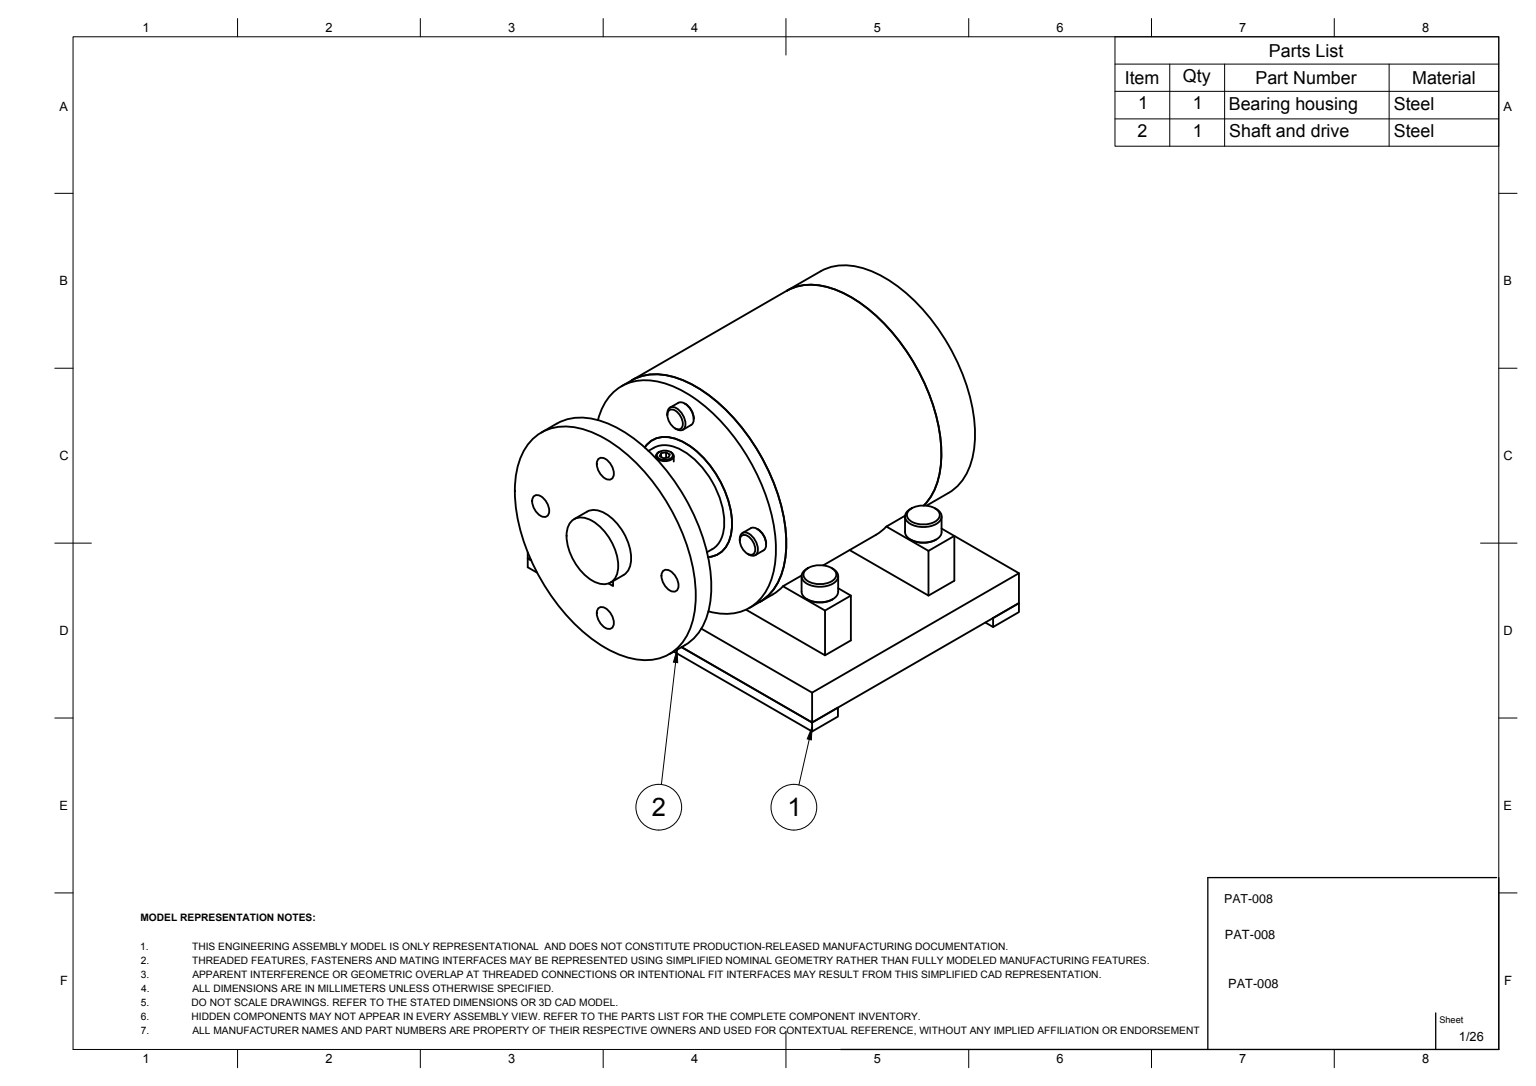
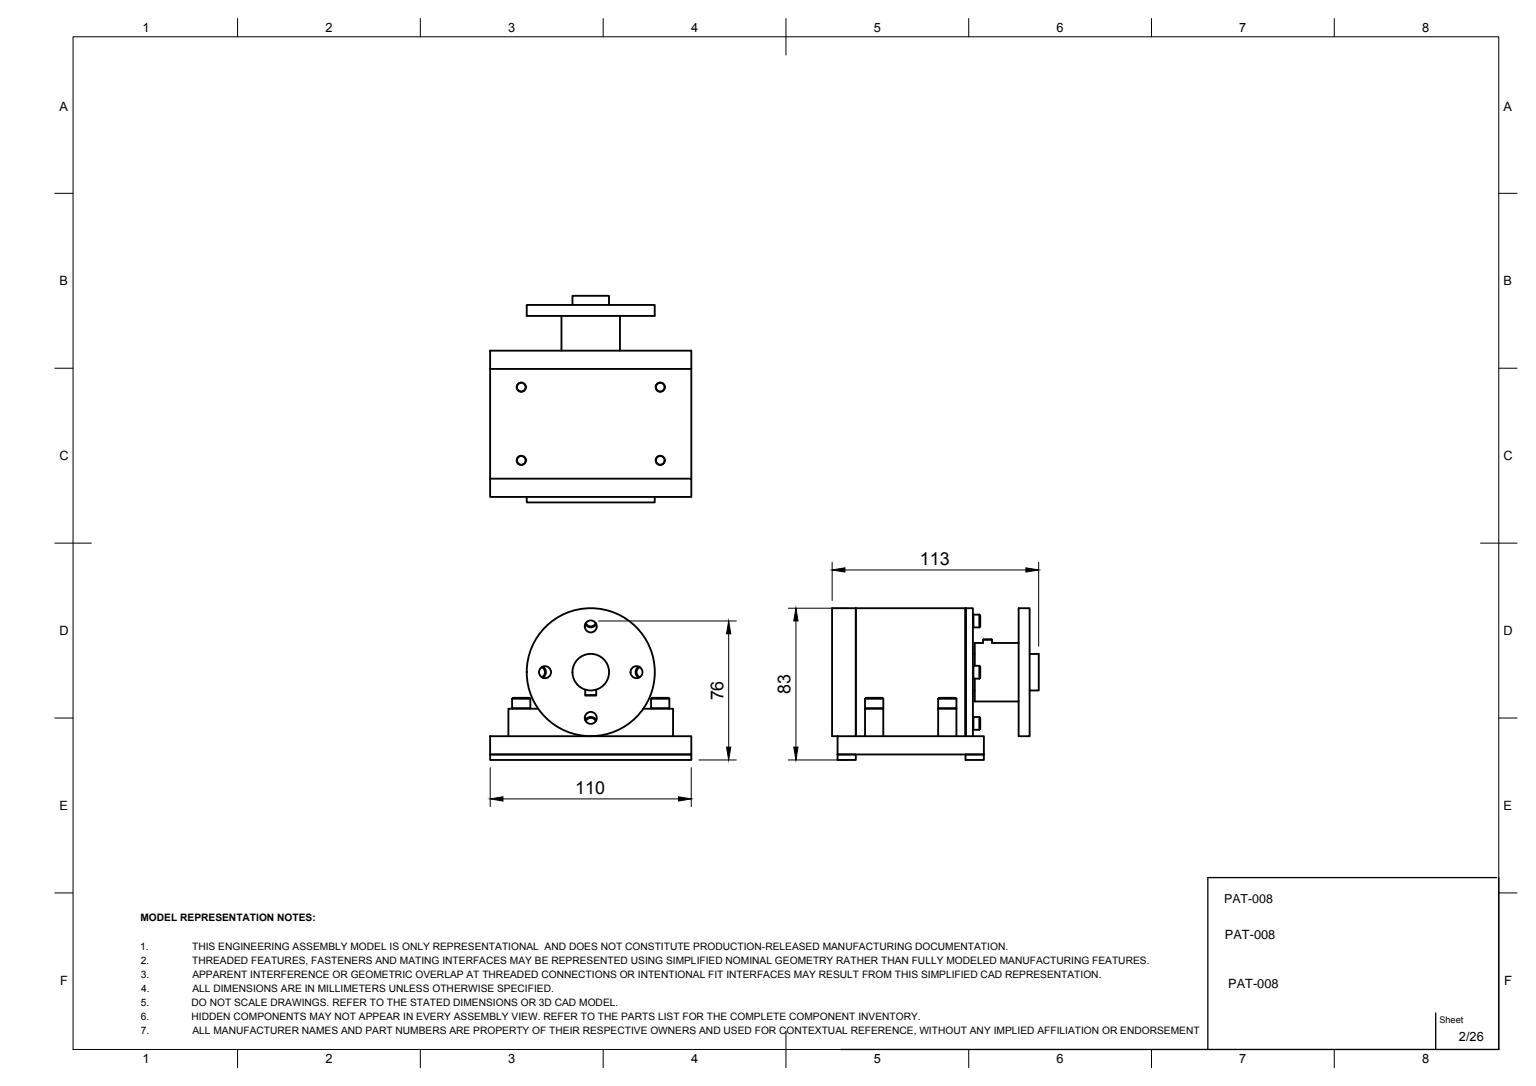
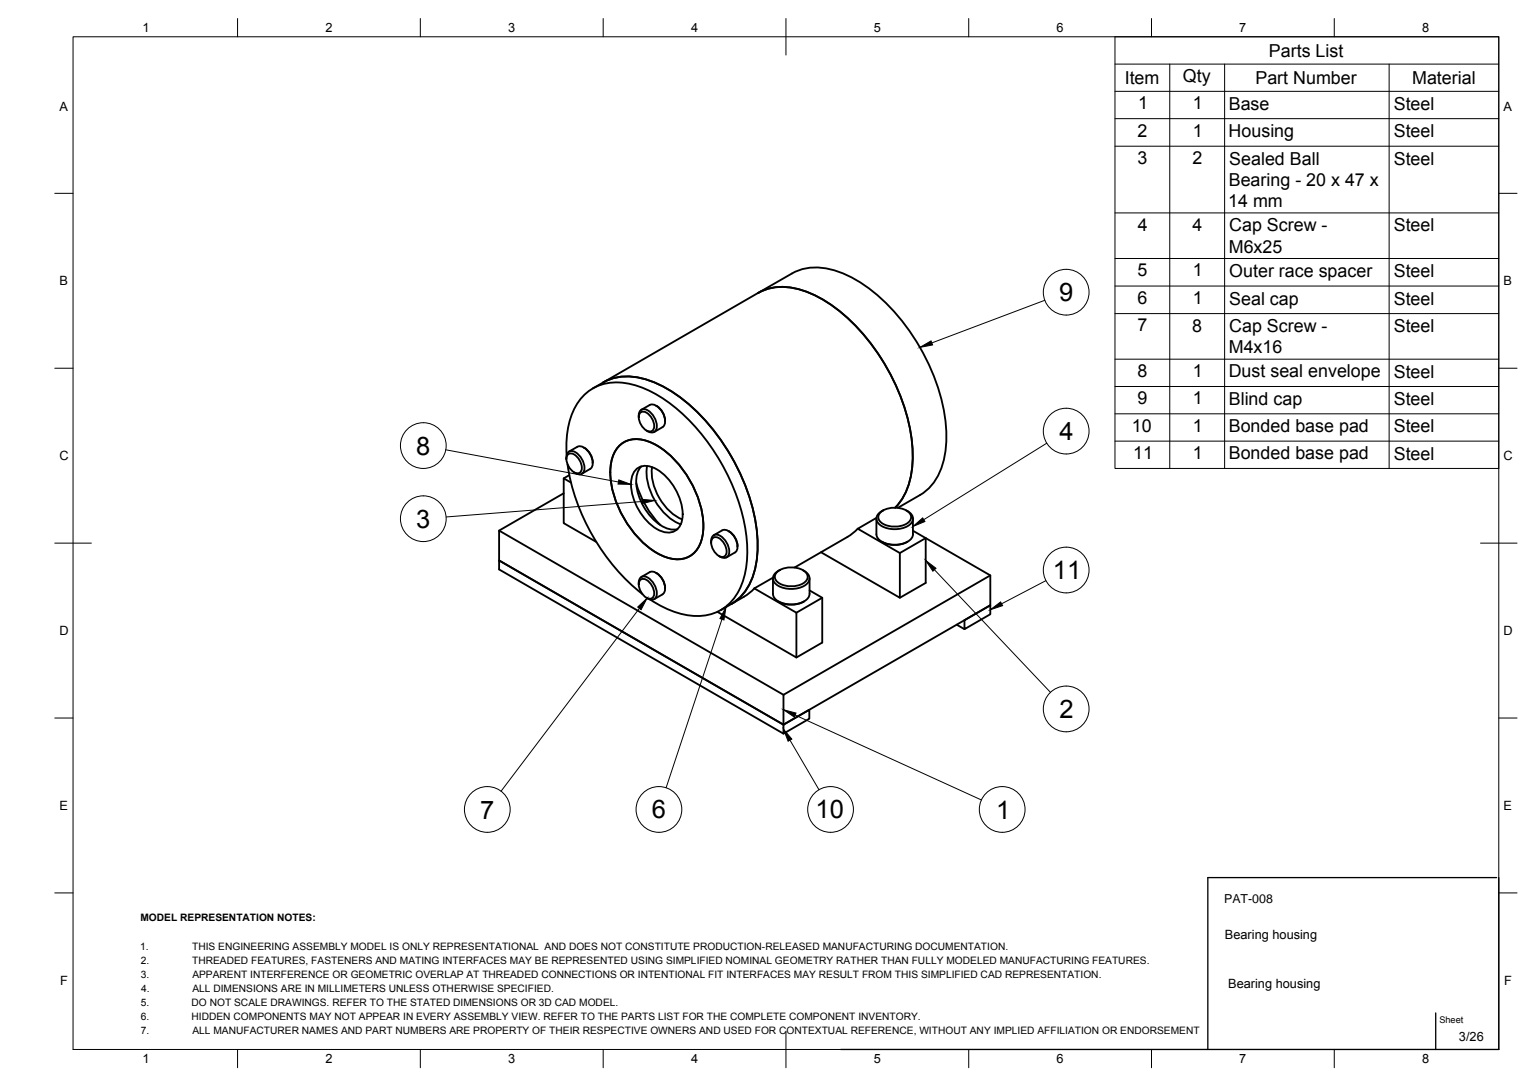
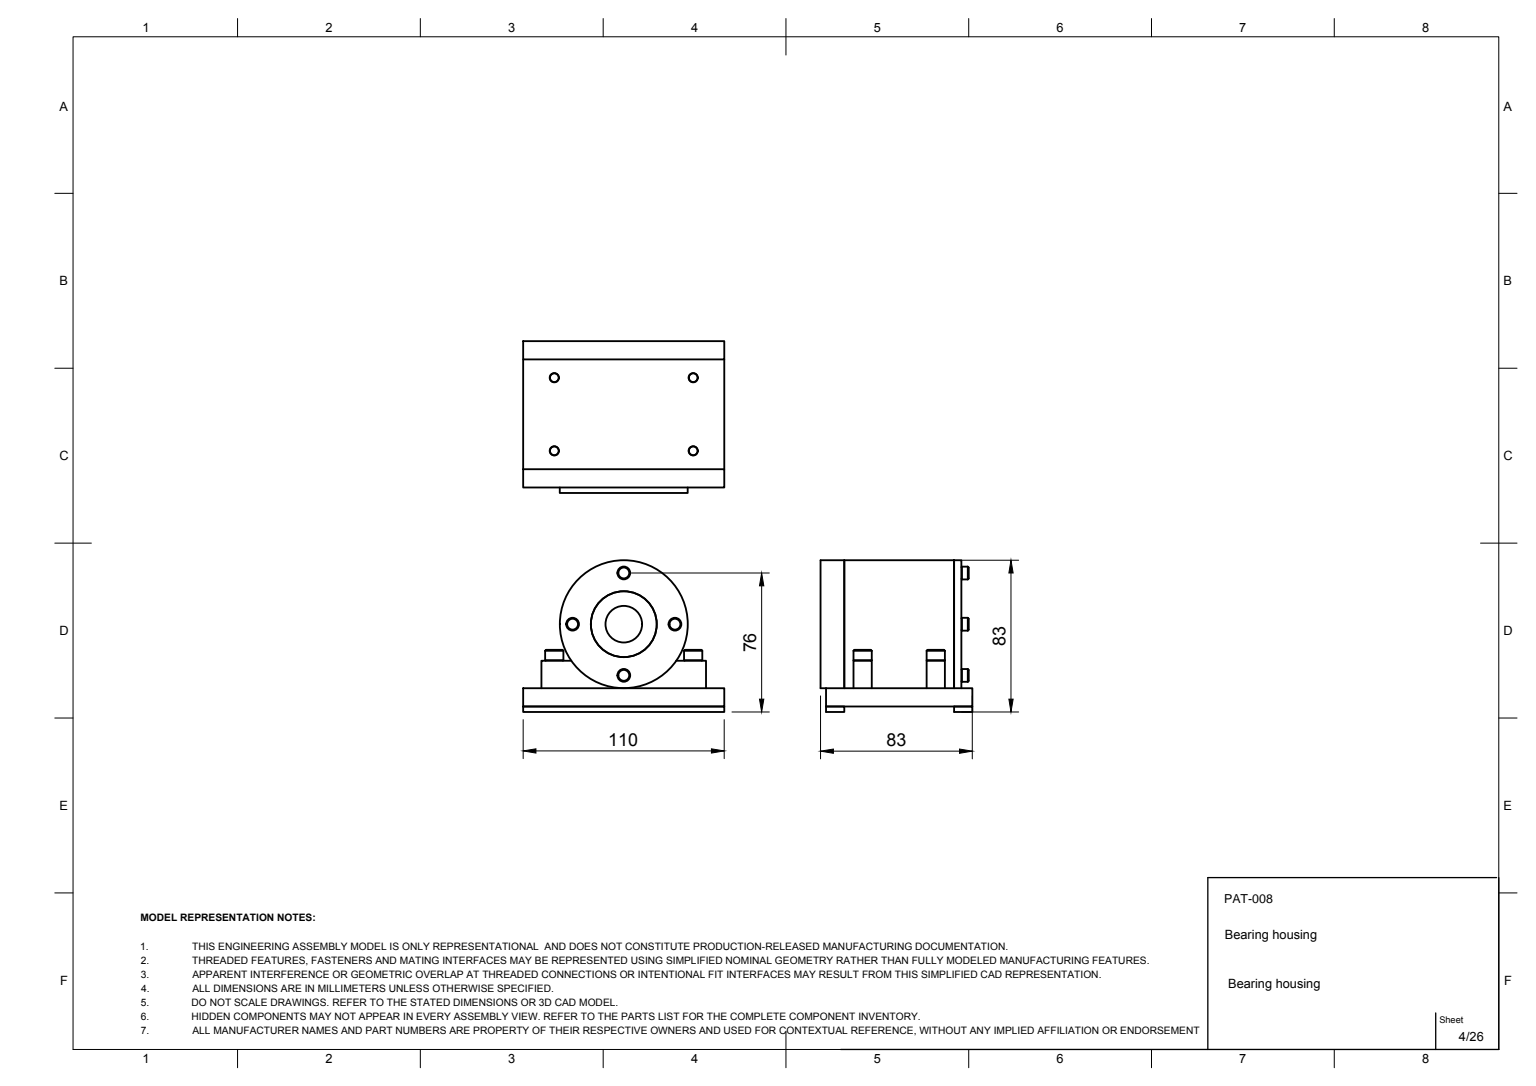
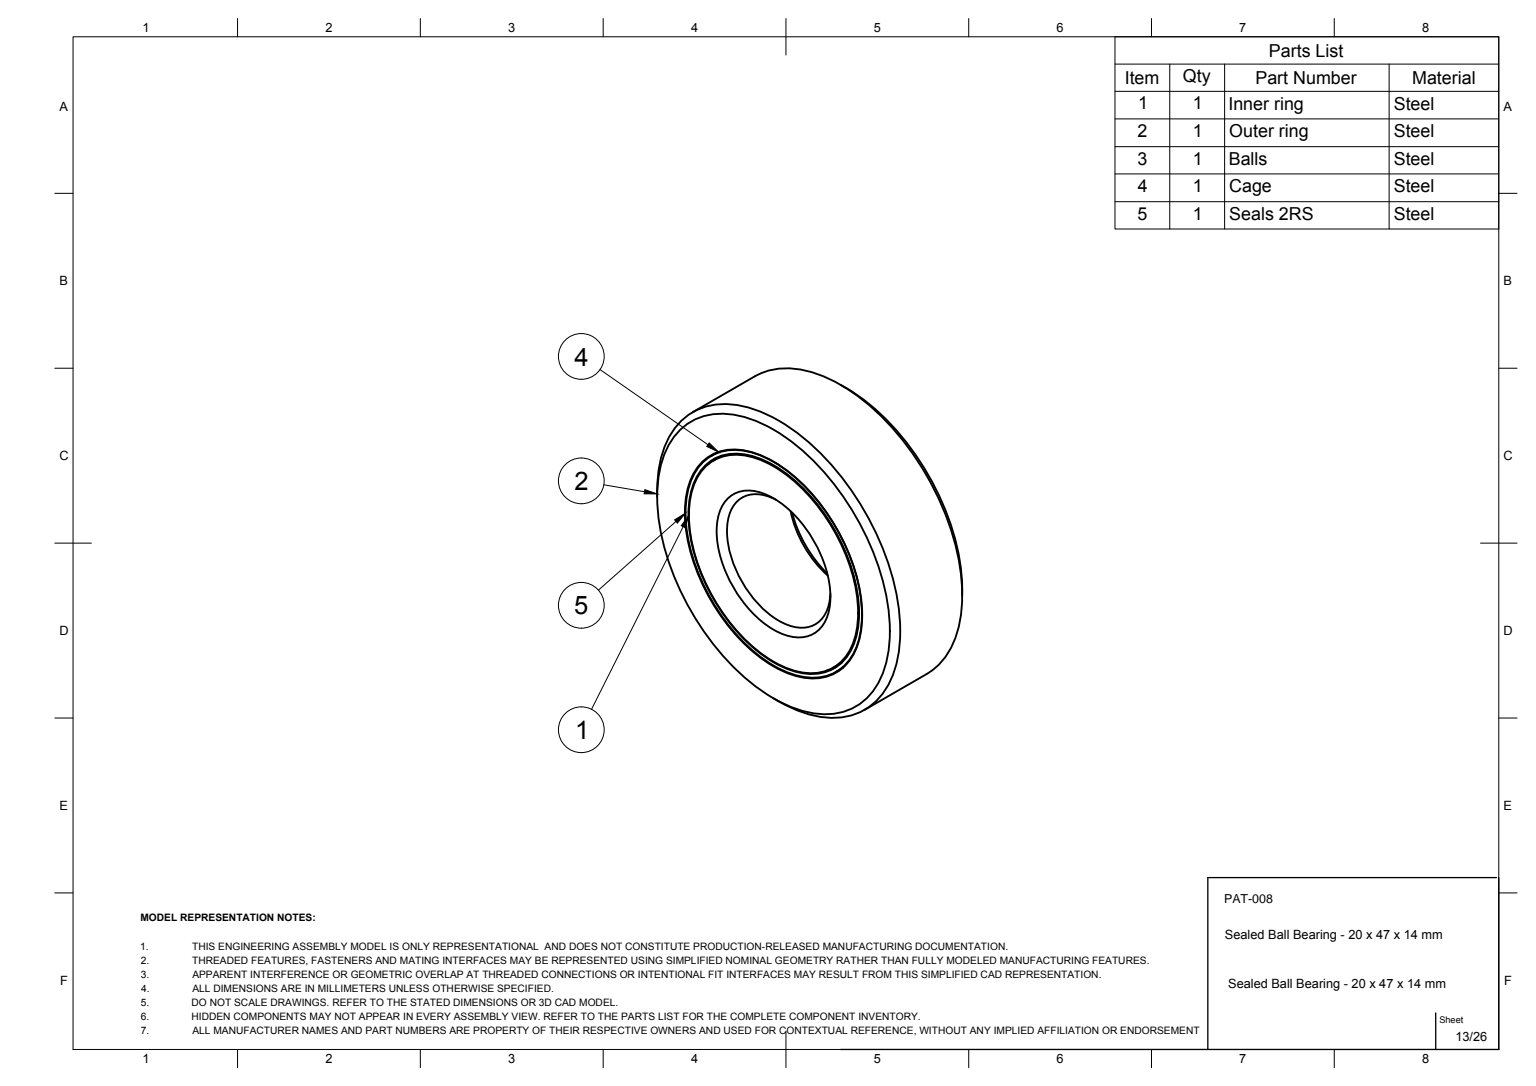
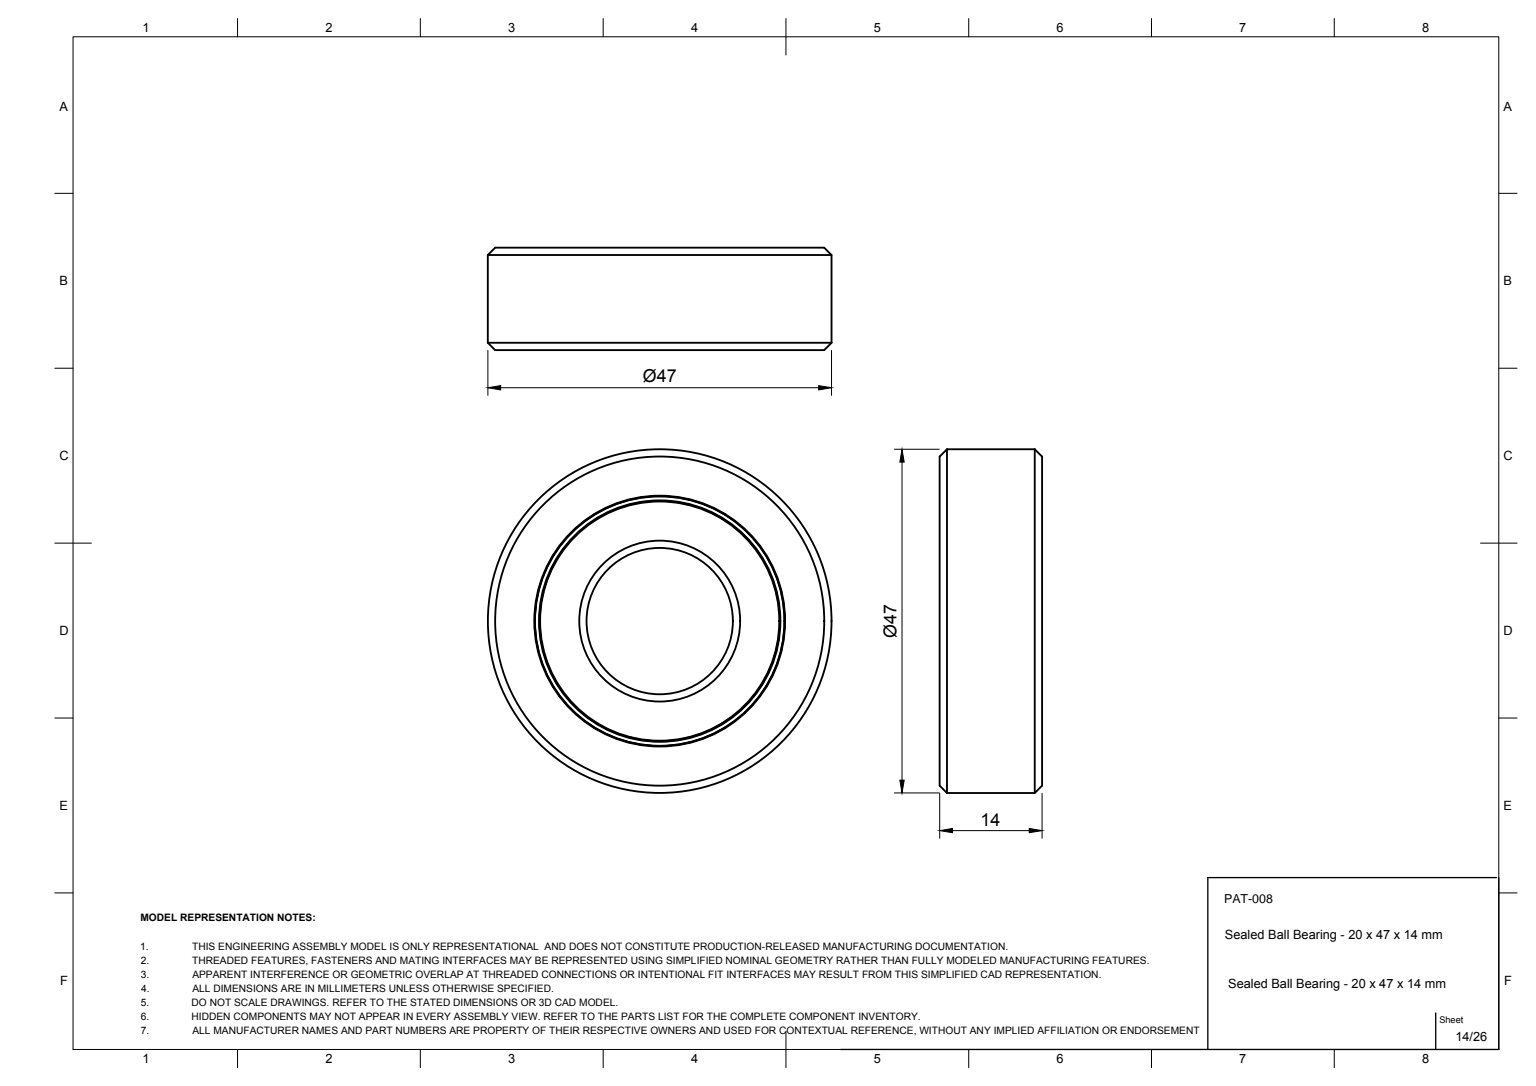
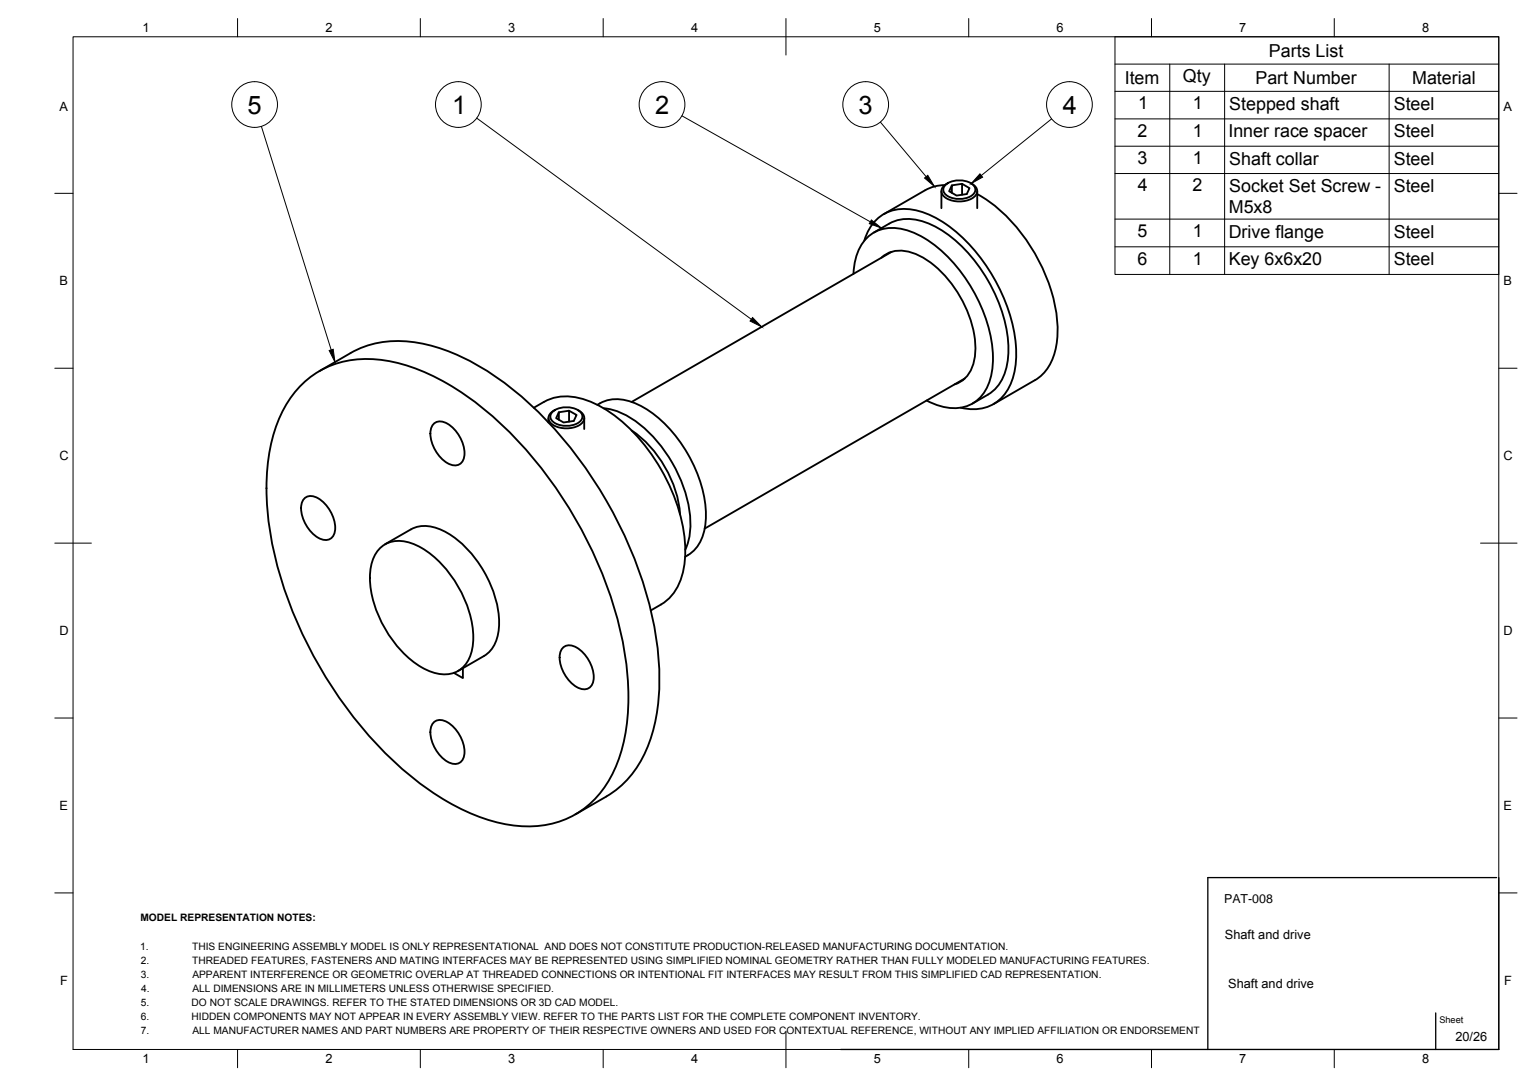
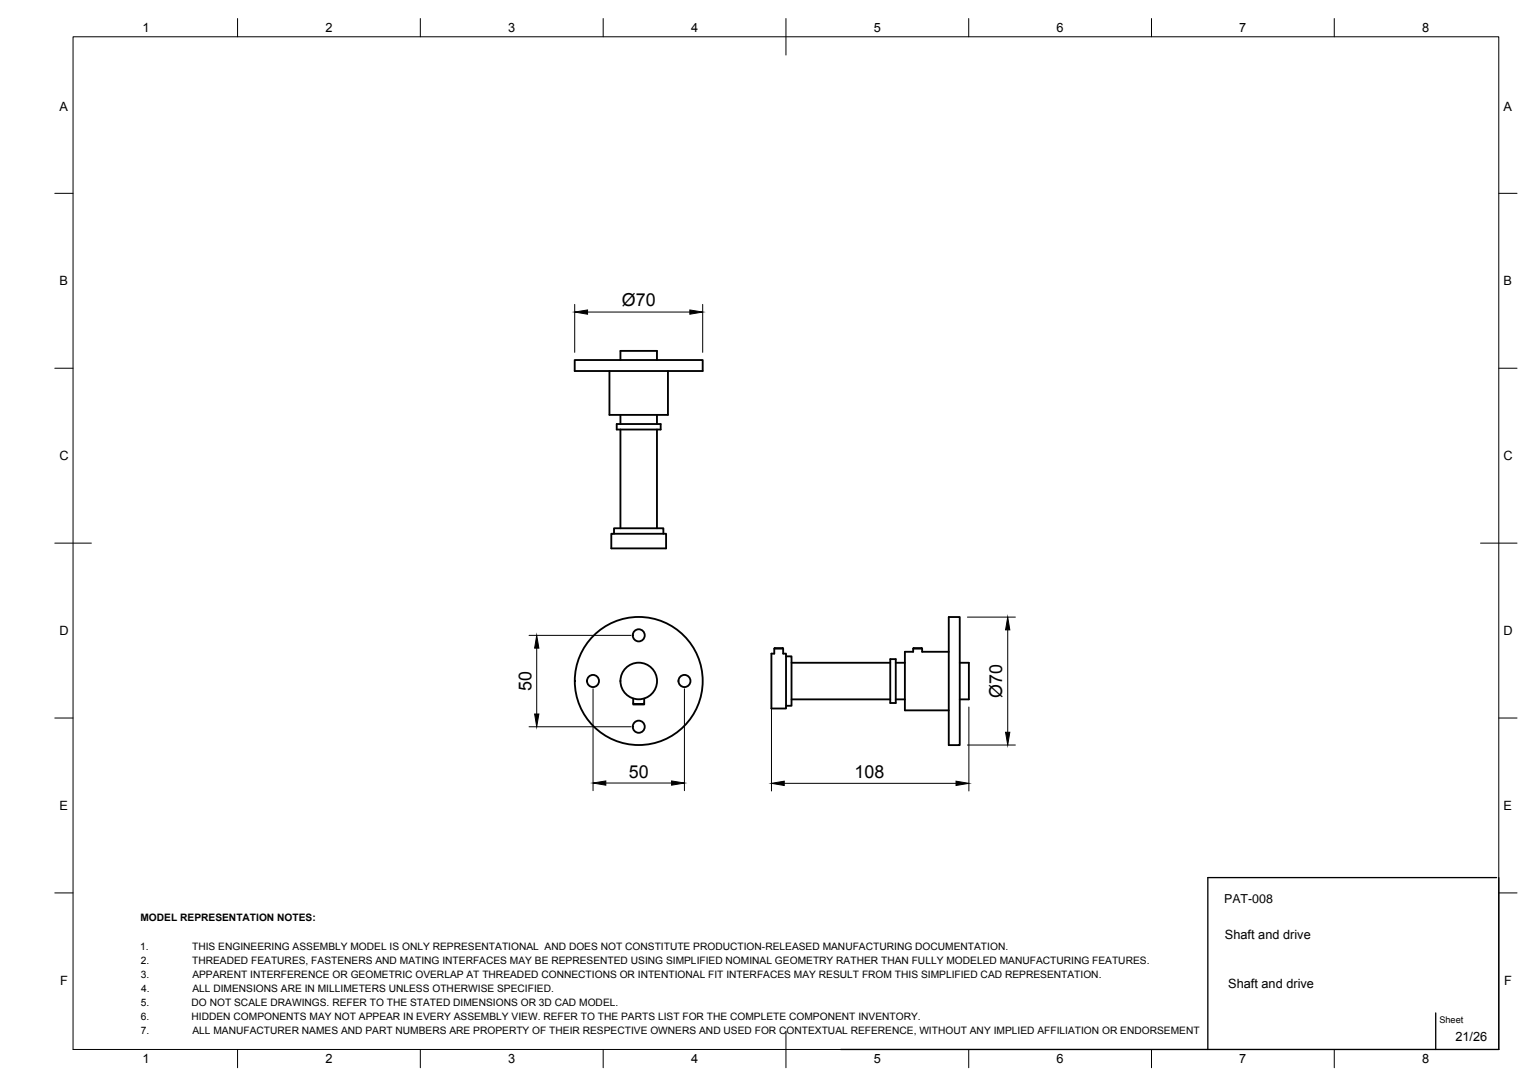
ISO-10303-21;
HEADER;
/* Generated by software containing ST-Developer
 * from STEP Tools, Inc. (www.steptools.com) 
 */

FILE_DESCRIPTION(
/* description */ ('Bearing housing with oil seal and end cap'),
/* implementation_level */ '2;1');

FILE_NAME(
/* name */ 'PAT-008',
/* time_stamp */ '2026-10-28T03:23:10-07:00',
/* author */ (''),
/* organization */ (''),
/* preprocessor_version */ 'ST-DEVELOPER v20.2',
/* originating_system */ 'Autodesk Translation Framework v15.17.0.0',
/* authorisation */ '');

FILE_SCHEMA (('AUTOMOTIVE_DESIGN { 1 0 10303 214 3 1 1 }'));
ENDSEC;

DATA;
#10=MECHANICAL_DESIGN_GEOMETRIC_PRESENTATION_REPRESENTATION('',(#259,#260,
#261,#262,#263,#264,#265,#266,#267,#268,#269,#270,#271,#272,#273,#274,#275,
#276,#277,#278,#279,#280,#281,#282,#283,#284,#285,#286,#287),#7871);
#11=ORIENTED_CLOSED_SHELL('',*,#4107,.F.);
#12=ORIENTED_CLOSED_SHELL('',*,#4109,.F.);
#13=BREP_WITH_VOIDS('Body1',#4106,(#11));
#14=BREP_WITH_VOIDS('Body1',#4108,(#12));
#15=ITEM_DEFINED_TRANSFORMATION($,$,#4556,#4684);
#16=ITEM_DEFINED_TRANSFORMATION($,$,#4576,#4685);
#17=ITEM_DEFINED_TRANSFORMATION($,$,#4596,#4686);
#18=ITEM_DEFINED_TRANSFORMATION($,$,#4613,#4687);
#19=ITEM_DEFINED_TRANSFORMATION($,$,#4667,#4688);
#20=ITEM_DEFINED_TRANSFORMATION($,$,#4350,#4741);
#21=ITEM_DEFINED_TRANSFORMATION($,$,#4369,#4742);
#22=ITEM_DEFINED_TRANSFORMATION($,$,#4448,#4743);
#23=ITEM_DEFINED_TRANSFORMATION($,$,#4457,#4744);
#24=ITEM_DEFINED_TRANSFORMATION($,$,#4486,#4745);
#25=ITEM_DEFINED_TRANSFORMATION($,$,#4495,#4746);
#26=ITEM_DEFINED_TRANSFORMATION($,$,#4541,#4747);
#27=ITEM_DEFINED_TRANSFORMATION($,$,#4548,#4748);
#28=ITEM_DEFINED_TRANSFORMATION($,$,#4555,#4749);
#29=ITEM_DEFINED_TRANSFORMATION($,$,#4689,#4750);
#30=ITEM_DEFINED_TRANSFORMATION($,$,#4689,#4751);
#31=ITEM_DEFINED_TRANSFORMATION($,$,#4555,#4752);
#32=ITEM_DEFINED_TRANSFORMATION($,$,#4689,#4753);
#33=ITEM_DEFINED_TRANSFORMATION($,$,#4689,#4754);
#34=ITEM_DEFINED_TRANSFORMATION($,$,#4715,#4755);
#35=ITEM_DEFINED_TRANSFORMATION($,$,#4715,#4756);
#36=ITEM_DEFINED_TRANSFORMATION($,$,#4715,#4757);
#37=ITEM_DEFINED_TRANSFORMATION($,$,#4715,#4758);
#38=ITEM_DEFINED_TRANSFORMATION($,$,#4715,#4759);
#39=ITEM_DEFINED_TRANSFORMATION($,$,#4715,#4760);
#40=ITEM_DEFINED_TRANSFORMATION($,$,#4715,#4761);
#41=ITEM_DEFINED_TRANSFORMATION($,$,#4715,#4762);
#42=ITEM_DEFINED_TRANSFORMATION($,$,#4764,#4871);
#43=ITEM_DEFINED_TRANSFORMATION($,$,#4785,#4872);
#44=ITEM_DEFINED_TRANSFORMATION($,$,#4794,#4873);
#45=ITEM_DEFINED_TRANSFORMATION($,$,#4809,#4874);
#46=ITEM_DEFINED_TRANSFORMATION($,$,#4854,#4875);
#47=ITEM_DEFINED_TRANSFORMATION($,$,#4843,#4876);
#48=ITEM_DEFINED_TRANSFORMATION($,$,#4854,#4877);
#49=ITEM_DEFINED_TRANSFORMATION($,$,#4349,#4878);
#50=ITEM_DEFINED_TRANSFORMATION($,$,#4763,#4879);
#51=(
REPRESENTATION_RELATIONSHIP($,$,#7973,#7972)
REPRESENTATION_RELATIONSHIP_WITH_TRANSFORMATION(#15)
SHAPE_REPRESENTATION_RELATIONSHIP()
);
#52=(
REPRESENTATION_RELATIONSHIP($,$,#7974,#7972)
REPRESENTATION_RELATIONSHIP_WITH_TRANSFORMATION(#16)
SHAPE_REPRESENTATION_RELATIONSHIP()
);
#53=(
REPRESENTATION_RELATIONSHIP($,$,#7975,#7972)
REPRESENTATION_RELATIONSHIP_WITH_TRANSFORMATION(#17)
SHAPE_REPRESENTATION_RELATIONSHIP()
);
#54=(
REPRESENTATION_RELATIONSHIP($,$,#7976,#7972)
REPRESENTATION_RELATIONSHIP_WITH_TRANSFORMATION(#18)
SHAPE_REPRESENTATION_RELATIONSHIP()
);
#55=(
REPRESENTATION_RELATIONSHIP($,$,#7977,#7972)
REPRESENTATION_RELATIONSHIP_WITH_TRANSFORMATION(#19)
SHAPE_REPRESENTATION_RELATIONSHIP()
);
#56=(
REPRESENTATION_RELATIONSHIP($,$,#7964,#7963)
REPRESENTATION_RELATIONSHIP_WITH_TRANSFORMATION(#20)
SHAPE_REPRESENTATION_RELATIONSHIP()
);
#57=(
REPRESENTATION_RELATIONSHIP($,$,#7965,#7963)
REPRESENTATION_RELATIONSHIP_WITH_TRANSFORMATION(#21)
SHAPE_REPRESENTATION_RELATIONSHIP()
);
#58=(
REPRESENTATION_RELATIONSHIP($,$,#7966,#7963)
REPRESENTATION_RELATIONSHIP_WITH_TRANSFORMATION(#22)
SHAPE_REPRESENTATION_RELATIONSHIP()
);
#59=(
REPRESENTATION_RELATIONSHIP($,$,#7967,#7963)
REPRESENTATION_RELATIONSHIP_WITH_TRANSFORMATION(#23)
SHAPE_REPRESENTATION_RELATIONSHIP()
);
#60=(
REPRESENTATION_RELATIONSHIP($,$,#7968,#7963)
REPRESENTATION_RELATIONSHIP_WITH_TRANSFORMATION(#24)
SHAPE_REPRESENTATION_RELATIONSHIP()
);
#61=(
REPRESENTATION_RELATIONSHIP($,$,#7969,#7963)
REPRESENTATION_RELATIONSHIP_WITH_TRANSFORMATION(#25)
SHAPE_REPRESENTATION_RELATIONSHIP()
);
#62=(
REPRESENTATION_RELATIONSHIP($,$,#7970,#7963)
REPRESENTATION_RELATIONSHIP_WITH_TRANSFORMATION(#26)
SHAPE_REPRESENTATION_RELATIONSHIP()
);
#63=(
REPRESENTATION_RELATIONSHIP($,$,#7971,#7963)
REPRESENTATION_RELATIONSHIP_WITH_TRANSFORMATION(#27)
SHAPE_REPRESENTATION_RELATIONSHIP()
);
#64=(
REPRESENTATION_RELATIONSHIP($,$,#7972,#7963)
REPRESENTATION_RELATIONSHIP_WITH_TRANSFORMATION(#28)
SHAPE_REPRESENTATION_RELATIONSHIP()
);
#65=(
REPRESENTATION_RELATIONSHIP($,$,#7978,#7963)
REPRESENTATION_RELATIONSHIP_WITH_TRANSFORMATION(#29)
SHAPE_REPRESENTATION_RELATIONSHIP()
);
#66=(
REPRESENTATION_RELATIONSHIP($,$,#7978,#7963)
REPRESENTATION_RELATIONSHIP_WITH_TRANSFORMATION(#30)
SHAPE_REPRESENTATION_RELATIONSHIP()
);
#67=(
REPRESENTATION_RELATIONSHIP($,$,#7972,#7963)
REPRESENTATION_RELATIONSHIP_WITH_TRANSFORMATION(#31)
SHAPE_REPRESENTATION_RELATIONSHIP()
);
#68=(
REPRESENTATION_RELATIONSHIP($,$,#7978,#7963)
REPRESENTATION_RELATIONSHIP_WITH_TRANSFORMATION(#32)
SHAPE_REPRESENTATION_RELATIONSHIP()
);
#69=(
REPRESENTATION_RELATIONSHIP($,$,#7978,#7963)
REPRESENTATION_RELATIONSHIP_WITH_TRANSFORMATION(#33)
SHAPE_REPRESENTATION_RELATIONSHIP()
);
#70=(
REPRESENTATION_RELATIONSHIP($,$,#7979,#7963)
REPRESENTATION_RELATIONSHIP_WITH_TRANSFORMATION(#34)
SHAPE_REPRESENTATION_RELATIONSHIP()
);
#71=(
REPRESENTATION_RELATIONSHIP($,$,#7979,#7963)
REPRESENTATION_RELATIONSHIP_WITH_TRANSFORMATION(#35)
SHAPE_REPRESENTATION_RELATIONSHIP()
);
#72=(
REPRESENTATION_RELATIONSHIP($,$,#7979,#7963)
REPRESENTATION_RELATIONSHIP_WITH_TRANSFORMATION(#36)
SHAPE_REPRESENTATION_RELATIONSHIP()
);
#73=(
REPRESENTATION_RELATIONSHIP($,$,#7979,#7963)
REPRESENTATION_RELATIONSHIP_WITH_TRANSFORMATION(#37)
SHAPE_REPRESENTATION_RELATIONSHIP()
);
#74=(
REPRESENTATION_RELATIONSHIP($,$,#7979,#7963)
REPRESENTATION_RELATIONSHIP_WITH_TRANSFORMATION(#38)
SHAPE_REPRESENTATION_RELATIONSHIP()
);
#75=(
REPRESENTATION_RELATIONSHIP($,$,#7979,#7963)
REPRESENTATION_RELATIONSHIP_WITH_TRANSFORMATION(#39)
SHAPE_REPRESENTATION_RELATIONSHIP()
);
#76=(
REPRESENTATION_RELATIONSHIP($,$,#7979,#7963)
REPRESENTATION_RELATIONSHIP_WITH_TRANSFORMATION(#40)
SHAPE_REPRESENTATION_RELATIONSHIP()
);
#77=(
REPRESENTATION_RELATIONSHIP($,$,#7979,#7963)
REPRESENTATION_RELATIONSHIP_WITH_TRANSFORMATION(#41)
SHAPE_REPRESENTATION_RELATIONSHIP()
);
#78=(
REPRESENTATION_RELATIONSHIP($,$,#7981,#7980)
REPRESENTATION_RELATIONSHIP_WITH_TRANSFORMATION(#42)
SHAPE_REPRESENTATION_RELATIONSHIP()
);
#79=(
REPRESENTATION_RELATIONSHIP($,$,#7982,#7980)
REPRESENTATION_RELATIONSHIP_WITH_TRANSFORMATION(#43)
SHAPE_REPRESENTATION_RELATIONSHIP()
);
#80=(
REPRESENTATION_RELATIONSHIP($,$,#7983,#7980)
REPRESENTATION_RELATIONSHIP_WITH_TRANSFORMATION(#44)
SHAPE_REPRESENTATION_RELATIONSHIP()
);
#81=(
REPRESENTATION_RELATIONSHIP($,$,#7984,#7980)
REPRESENTATION_RELATIONSHIP_WITH_TRANSFORMATION(#45)
SHAPE_REPRESENTATION_RELATIONSHIP()
);
#82=(
REPRESENTATION_RELATIONSHIP($,$,#7986,#7980)
REPRESENTATION_RELATIONSHIP_WITH_TRANSFORMATION(#46)
SHAPE_REPRESENTATION_RELATIONSHIP()
);
#83=(
REPRESENTATION_RELATIONSHIP($,$,#7985,#7980)
REPRESENTATION_RELATIONSHIP_WITH_TRANSFORMATION(#47)
SHAPE_REPRESENTATION_RELATIONSHIP()
);
#84=(
REPRESENTATION_RELATIONSHIP($,$,#7986,#7980)
REPRESENTATION_RELATIONSHIP_WITH_TRANSFORMATION(#48)
SHAPE_REPRESENTATION_RELATIONSHIP()
);
#85=(
REPRESENTATION_RELATIONSHIP($,$,#7963,#7962)
REPRESENTATION_RELATIONSHIP_WITH_TRANSFORMATION(#49)
SHAPE_REPRESENTATION_RELATIONSHIP()
);
#86=(
REPRESENTATION_RELATIONSHIP($,$,#7980,#7962)
REPRESENTATION_RELATIONSHIP_WITH_TRANSFORMATION(#50)
SHAPE_REPRESENTATION_RELATIONSHIP()
);
#87=CONTEXT_DEPENDENT_SHAPE_REPRESENTATION(#51,#7917);
#88=CONTEXT_DEPENDENT_SHAPE_REPRESENTATION(#52,#7918);
#89=CONTEXT_DEPENDENT_SHAPE_REPRESENTATION(#53,#7919);
#90=CONTEXT_DEPENDENT_SHAPE_REPRESENTATION(#54,#7920);
#91=CONTEXT_DEPENDENT_SHAPE_REPRESENTATION(#55,#7921);
#92=CONTEXT_DEPENDENT_SHAPE_REPRESENTATION(#56,#7924);
#93=CONTEXT_DEPENDENT_SHAPE_REPRESENTATION(#57,#7925);
#94=CONTEXT_DEPENDENT_SHAPE_REPRESENTATION(#58,#7926);
#95=CONTEXT_DEPENDENT_SHAPE_REPRESENTATION(#59,#7927);
#96=CONTEXT_DEPENDENT_SHAPE_REPRESENTATION(#60,#7928);
#97=CONTEXT_DEPENDENT_SHAPE_REPRESENTATION(#61,#7929);
#98=CONTEXT_DEPENDENT_SHAPE_REPRESENTATION(#62,#7930);
#99=CONTEXT_DEPENDENT_SHAPE_REPRESENTATION(#63,#7931);
#100=CONTEXT_DEPENDENT_SHAPE_REPRESENTATION(#64,#7932);
#101=CONTEXT_DEPENDENT_SHAPE_REPRESENTATION(#65,#7933);
#102=CONTEXT_DEPENDENT_SHAPE_REPRESENTATION(#66,#7934);
#103=CONTEXT_DEPENDENT_SHAPE_REPRESENTATION(#67,#7935);
#104=CONTEXT_DEPENDENT_SHAPE_REPRESENTATION(#68,#7936);
#105=CONTEXT_DEPENDENT_SHAPE_REPRESENTATION(#69,#7937);
#106=CONTEXT_DEPENDENT_SHAPE_REPRESENTATION(#70,#7938);
#107=CONTEXT_DEPENDENT_SHAPE_REPRESENTATION(#71,#7939);
#108=CONTEXT_DEPENDENT_SHAPE_REPRESENTATION(#72,#7940);
#109=CONTEXT_DEPENDENT_SHAPE_REPRESENTATION(#73,#7941);
#110=CONTEXT_DEPENDENT_SHAPE_REPRESENTATION(#74,#7942);
#111=CONTEXT_DEPENDENT_SHAPE_REPRESENTATION(#75,#7943);
#112=CONTEXT_DEPENDENT_SHAPE_REPRESENTATION(#76,#7944);
#113=CONTEXT_DEPENDENT_SHAPE_REPRESENTATION(#77,#7945);
#114=CONTEXT_DEPENDENT_SHAPE_REPRESENTATION(#78,#7953);
#115=CONTEXT_DEPENDENT_SHAPE_REPRESENTATION(#79,#7954);
#116=CONTEXT_DEPENDENT_SHAPE_REPRESENTATION(#80,#7955);
#117=CONTEXT_DEPENDENT_SHAPE_REPRESENTATION(#81,#7956);
#118=CONTEXT_DEPENDENT_SHAPE_REPRESENTATION(#82,#7957);
#119=CONTEXT_DEPENDENT_SHAPE_REPRESENTATION(#83,#7958);
#120=CONTEXT_DEPENDENT_SHAPE_REPRESENTATION(#84,#7959);
#121=CONTEXT_DEPENDENT_SHAPE_REPRESENTATION(#85,#7960);
#122=CONTEXT_DEPENDENT_SHAPE_REPRESENTATION(#86,#7961);
#123=NEXT_ASSEMBLY_USAGE_OCCURRENCE('Inner ring:1','Inner ring:1',
'Inner ring:1',#7998,#7999,'Inner ring:1');
#124=NEXT_ASSEMBLY_USAGE_OCCURRENCE('Outer ring:1','Outer ring:1',
'Outer ring:1',#7998,#8000,'Outer ring:1');
#125=NEXT_ASSEMBLY_USAGE_OCCURRENCE('Balls:1','Balls:1','Balls:1',#7998,
#8001,'Balls:1');
#126=NEXT_ASSEMBLY_USAGE_OCCURRENCE('Cage:1','Cage:1','Cage:1',#7998,#8002,
'Cage:1');
#127=NEXT_ASSEMBLY_USAGE_OCCURRENCE('Seals 2RS:1','Seals 2RS:1',
'Seals 2RS:1',#7998,#8003,'Seals 2RS:1');
#128=NEXT_ASSEMBLY_USAGE_OCCURRENCE('Base:1','Base:1','Base:1',#7989,#7990,
'Base:1');
#129=NEXT_ASSEMBLY_USAGE_OCCURRENCE('Housing:1','Housing:1','Housing:1',
#7989,#7991,'Housing:1');
#130=NEXT_ASSEMBLY_USAGE_OCCURRENCE('Outer race spacer:1',
'Outer race spacer:1','Outer race spacer:1',#7989,#7992,
'Outer race spacer:1');
#131=NEXT_ASSEMBLY_USAGE_OCCURRENCE('Seal cap:1','Seal cap:1',
'Seal cap:1',#7989,#7993,'Seal cap:1');
#132=NEXT_ASSEMBLY_USAGE_OCCURRENCE('Dust seal envelope:1',
'Dust seal envelope:1','Dust seal envelope:1',#7989,#7994,
'Dust seal envelope:1');
#133=NEXT_ASSEMBLY_USAGE_OCCURRENCE('Blind cap:1','Blind cap:1',
'Blind cap:1',#7989,#7995,'Blind cap:1');
#134=NEXT_ASSEMBLY_USAGE_OCCURRENCE('Bonded base pad:1',
'Bonded base pad:1','Bonded base pad:1',#7989,#7996,'Bonded base pad:1');
#135=NEXT_ASSEMBLY_USAGE_OCCURRENCE('Bonded base pad (1):1',
'Bonded base pad (1):1','Bonded base pad (1):1',#7989,#7997,
'Bonded base pad (1):1');
#136=NEXT_ASSEMBLY_USAGE_OCCURRENCE(
'Sealed Ball Bearing - 20 x 47 x 14 mm:2',
'Sealed Ball Bearing - 20 x 47 x 14 mm:2',
'Sealed Ball Bearing - 20 x 47 x 14 mm:2',#7989,#7998,
'Sealed Ball Bearing - 20 x 47 x 14 mm:2');
#137=NEXT_ASSEMBLY_USAGE_OCCURRENCE('Cap Screw - M6x25:2',
'Cap Screw - M6x25:2','Cap Screw - M6x25:2',#7989,#8004,
'Cap Screw - M6x25:2');
#138=NEXT_ASSEMBLY_USAGE_OCCURRENCE('Cap Screw - M6x25:3',
'Cap Screw - M6x25:3','Cap Screw - M6x25:3',#7989,#8004,
'Cap Screw - M6x25:3');
#139=NEXT_ASSEMBLY_USAGE_OCCURRENCE(
'Sealed Ball Bearing - 20 x 47 x 14 mm:3',
'Sealed Ball Bearing - 20 x 47 x 14 mm:3',
'Sealed Ball Bearing - 20 x 47 x 14 mm:3',#7989,#7998,
'Sealed Ball Bearing - 20 x 47 x 14 mm:3');
#140=NEXT_ASSEMBLY_USAGE_OCCURRENCE('Cap Screw - M6x25:4',
'Cap Screw - M6x25:4','Cap Screw - M6x25:4',#7989,#8004,
'Cap Screw - M6x25:4');
#141=NEXT_ASSEMBLY_USAGE_OCCURRENCE('Cap Screw - M6x25:5',
'Cap Screw - M6x25:5','Cap Screw - M6x25:5',#7989,#8004,
'Cap Screw - M6x25:5');
#142=NEXT_ASSEMBLY_USAGE_OCCURRENCE('Cap Screw - M4x16:2',
'Cap Screw - M4x16:2','Cap Screw - M4x16:2',#7989,#8005,
'Cap Screw - M4x16:2');
#143=NEXT_ASSEMBLY_USAGE_OCCURRENCE('Cap Screw - M4x16:3',
'Cap Screw - M4x16:3','Cap Screw - M4x16:3',#7989,#8005,
'Cap Screw - M4x16:3');
#144=NEXT_ASSEMBLY_USAGE_OCCURRENCE('Cap Screw - M4x16:4',
'Cap Screw - M4x16:4','Cap Screw - M4x16:4',#7989,#8005,
'Cap Screw - M4x16:4');
#145=NEXT_ASSEMBLY_USAGE_OCCURRENCE('Cap Screw - M4x16:5',
'Cap Screw - M4x16:5','Cap Screw - M4x16:5',#7989,#8005,
'Cap Screw - M4x16:5');
#146=NEXT_ASSEMBLY_USAGE_OCCURRENCE('Cap Screw - M4x16:6',
'Cap Screw - M4x16:6','Cap Screw - M4x16:6',#7989,#8005,
'Cap Screw - M4x16:6');
#147=NEXT_ASSEMBLY_USAGE_OCCURRENCE('Cap Screw - M4x16:7',
'Cap Screw - M4x16:7','Cap Screw - M4x16:7',#7989,#8005,
'Cap Screw - M4x16:7');
#148=NEXT_ASSEMBLY_USAGE_OCCURRENCE('Cap Screw - M4x16:8',
'Cap Screw - M4x16:8','Cap Screw - M4x16:8',#7989,#8005,
'Cap Screw - M4x16:8');
#149=NEXT_ASSEMBLY_USAGE_OCCURRENCE('Cap Screw - M4x16:9',
'Cap Screw - M4x16:9','Cap Screw - M4x16:9',#7989,#8005,
'Cap Screw - M4x16:9');
#150=NEXT_ASSEMBLY_USAGE_OCCURRENCE('Stepped shaft:1','Stepped shaft:1',
'Stepped shaft:1',#8006,#8007,'Stepped shaft:1');
#151=NEXT_ASSEMBLY_USAGE_OCCURRENCE('Inner race spacer:1',
'Inner race spacer:1','Inner race spacer:1',#8006,#8008,
'Inner race spacer:1');
#152=NEXT_ASSEMBLY_USAGE_OCCURRENCE('Shaft collar:1','Shaft collar:1',
'Shaft collar:1',#8006,#8009,'Shaft collar:1');
#153=NEXT_ASSEMBLY_USAGE_OCCURRENCE('Drive flange:1','Drive flange:1',
'Drive flange:1',#8006,#8010,'Drive flange:1');
#154=NEXT_ASSEMBLY_USAGE_OCCURRENCE('Socket Set Screw - M5x8:2',
'Socket Set Screw - M5x8:2','Socket Set Screw - M5x8:2',#8006,#8012,
'Socket Set Screw - M5x8:2');
#155=NEXT_ASSEMBLY_USAGE_OCCURRENCE('Key 6x6x20:2','Key 6x6x20:2',
'Key 6x6x20:2',#8006,#8011,'Key 6x6x20:2');
#156=NEXT_ASSEMBLY_USAGE_OCCURRENCE('Socket Set Screw - M5x8:3',
'Socket Set Screw - M5x8:3','Socket Set Screw - M5x8:3',#8006,#8012,
'Socket Set Screw - M5x8:3');
#157=NEXT_ASSEMBLY_USAGE_OCCURRENCE('Bearing housing:1',
'Bearing housing:1','Bearing housing:1',#7988,#7989,'Bearing housing:1');
#158=NEXT_ASSEMBLY_USAGE_OCCURRENCE('Shaft and drive:1',
'Shaft and drive:1','Shaft and drive:1',#7988,#8006,'Shaft and drive:1');
#159=B_SPLINE_CURVE_WITH_KNOTS('',3,(#6771,#6772,#6773,#6774,#6775,#6776,
#6777,#6778,#6779,#6780,#6781,#6782,#6783,#6784,#6785,#6786,#6787,#6788,
#6789,#6790,#6791,#6792),.UNSPECIFIED.,.F.,.F.,(4,2,2,2,2,2,2,2,2,2,4),
(0.0789094028588958,0.210573405340968,0.315860108011452,0.421146810681936,
0.522142632548711,0.623138454415485,0.72413427628226,0.825130098149035,
0.930416800819519,1.03570350349,1.16736750597208),.UNSPECIFIED.);
#160=B_SPLINE_CURVE_WITH_KNOTS('',3,(#6796,#6797,#6798,#6799,#6800,#6801,
#6802,#6803,#6804,#6805,#6806,#6807,#6808,#6809,#6810,#6811,#6812,#6813,
#6814,#6815,#6816,#6817),.UNSPECIFIED.,.F.,.F.,(4,2,2,2,2,2,2,2,2,2,4),
(0.0774793363974613,0.142088896491891,0.284177792983782,0.411119756996526,
0.514392970548519,0.617666184100513,0.720939397652506,0.8242126112045,0.951154575217244,
1.09324347170913,1.15785303180356),.UNSPECIFIED.);
#161=B_SPLINE_CURVE_WITH_KNOTS('',3,(#6823,#6824,#6825,#6826,#6827,#6828,
#6829,#6830,#6831,#6832,#6833,#6834,#6835,#6836,#6837,#6838,#6839,#6840,
#6841,#6842,#6843,#6844),.UNSPECIFIED.,.F.,.F.,(4,2,2,2,2,2,2,2,2,2,4),
(0.0774793363974613,0.142088896491891,0.284177792983782,0.411119756996525,
0.514392970548519,0.617666184100513,0.720939397652506,0.8242126112045,0.951154575217243,
1.09324347170913,1.15785303180356),.UNSPECIFIED.);
#162=B_SPLINE_CURVE_WITH_KNOTS('',3,(#6848,#6849,#6850,#6851,#6852,#6853,
#6854,#6855,#6856,#6857,#6858,#6859,#6860,#6861,#6862,#6863,#6864,#6865,
#6866,#6867,#6868,#6869),.UNSPECIFIED.,.F.,.F.,(4,2,2,2,2,2,2,2,2,2,4),
(0.0774793363974614,0.142088896491891,0.284177792983781,0.411119756996525,
0.514392970548519,0.617666184100512,0.720939397652506,0.824212611204499,
0.951154575217243,1.09324347170913,1.15785303180356),.UNSPECIFIED.);
#163=B_SPLINE_CURVE_WITH_KNOTS('',3,(#6873,#6874,#6875,#6876,#6877,#6878,
#6879,#6880,#6881,#6882,#6883,#6884),.UNSPECIFIED.,.F.,.F.,(4,2,2,2,2,4),
(0.0774793363974613,0.142088896491891,0.284177792983781,0.411119756996525,
0.514392970548519,0.617666184100512),.UNSPECIFIED.);
#164=B_SPLINE_CURVE_WITH_KNOTS('',3,(#6889,#6890,#6891,#6892,#6893,#6894,
#6895,#6896,#6897,#6898,#6899,#6900),.UNSPECIFIED.,.F.,.F.,(4,2,2,2,2,4),
(0.617666184100512,0.720939397652506,0.824212611204499,0.951154575217243,
1.09324347170913,1.15785303180356),.UNSPECIFIED.);
#165=B_SPLINE_CURVE_WITH_KNOTS('',3,(#6904,#6905,#6906,#6907,#6908,#6909,
#6910,#6911,#6912,#6913,#6914,#6915,#6916,#6917,#6918,#6919,#6920,#6921,
#6922,#6923,#6924,#6925),.UNSPECIFIED.,.F.,.F.,(4,2,2,2,2,2,2,2,2,2,4),
(0.0774793363974613,0.142088896491891,0.284177792983782,0.411119756996526,
0.514392970548519,0.617666184100513,0.720939397652507,0.8242126112045,0.951154575217245,
1.09324347170914,1.15785303180356),.UNSPECIFIED.);
#166=B_SPLINE_CURVE_WITH_KNOTS('',3,(#6929,#6930,#6931,#6932,#6933,#6934,
#6935,#6936,#6937,#6938,#6939,#6940,#6941,#6942,#6943,#6944,#6945,#6946,
#6947,#6948,#6949,#6950),.UNSPECIFIED.,.F.,.F.,(4,2,2,2,2,2,2,2,2,2,4),
(0.0774793363974613,0.142088896491891,0.284177792983782,0.411119756996526,
0.514392970548519,0.617666184100513,0.720939397652506,0.824212611204499,
0.951154575217243,1.09324347170913,1.15785303180356),.UNSPECIFIED.);
#167=B_SPLINE_CURVE_WITH_KNOTS('',3,(#6954,#6955,#6956,#6957,#6958,#6959,
#6960,#6961,#6962,#6963,#6964,#6965,#6966,#6967,#6968,#6969,#6970,#6971,
#6972,#6973,#6974,#6975),.UNSPECIFIED.,.F.,.F.,(4,2,2,2,2,2,2,2,2,2,4),
(0.0774793363974613,0.142088896491891,0.284177792983782,0.411119756996526,
0.514392970548519,0.617666184100513,0.720939397652506,0.8242126112045,0.951154575217244,
1.09324347170913,1.15785303180356),.UNSPECIFIED.);
#168=B_SPLINE_CURVE_WITH_KNOTS('',3,(#6979,#6980,#6981,#6982,#6983,#6984,
#6985,#6986,#6987,#6988,#6989,#6990,#6991,#6992,#6993,#6994,#6995,#6996,
#6997,#6998,#6999,#7000),.UNSPECIFIED.,.F.,.F.,(4,2,2,2,2,2,2,2,2,2,4),
(0.0774793363974613,0.142088896491891,0.284177792983782,0.411119756996526,
0.514392970548519,0.617666184100513,0.720939397652506,0.8242126112045,0.951154575217243,
1.09324347170913,1.15785303180356),.UNSPECIFIED.);
#169=B_SPLINE_CURVE_WITH_KNOTS('',3,(#7008,#7009,#7010,#7011,#7012,#7013,
#7014,#7015,#7016,#7017,#7018,#7019,#7020,#7021,#7022,#7023,#7024,#7025,
#7026,#7027,#7028,#7029),.UNSPECIFIED.,.F.,.F.,(4,2,2,2,2,2,2,2,2,2,4),
(0.0789094028588958,0.210573405340968,0.315860108011452,0.421146810681936,
0.522142632548711,0.623138454415485,0.72413427628226,0.825130098149035,
0.930416800819519,1.03570350349,1.16736750597208),.UNSPECIFIED.);
#170=B_SPLINE_CURVE_WITH_KNOTS('',3,(#7037,#7038,#7039,#7040,#7041,#7042,
#7043,#7044,#7045,#7046,#7047,#7048,#7049,#7050,#7051,#7052,#7053,#7054,
#7055,#7056,#7057,#7058),.UNSPECIFIED.,.F.,.F.,(4,2,2,2,2,2,2,2,2,2,4),
(0.0789094028588958,0.210573405340969,0.315860108011453,0.421146810681937,
0.522142632548712,0.623138454415486,0.724134276282261,0.825130098149035,
0.930416800819519,1.03570350349,1.16736750597208),.UNSPECIFIED.);
#171=B_SPLINE_CURVE_WITH_KNOTS('',3,(#7067,#7068,#7069,#7070,#7071,#7072,
#7073,#7074,#7075,#7076,#7077,#7078),.UNSPECIFIED.,.F.,.F.,(4,2,2,2,2,4),
(0.0789094028588958,0.210573405340968,0.315860108011452,0.421146810681937,
0.522142632548711,0.623138454415486),.UNSPECIFIED.);
#172=B_SPLINE_CURVE_WITH_KNOTS('',3,(#7080,#7081,#7082,#7083,#7084,#7085,
#7086,#7087,#7088,#7089,#7090,#7091),.UNSPECIFIED.,.F.,.F.,(4,2,2,2,2,4),
(0.623138454415486,0.72413427628226,0.825130098149035,0.930416800819519,
1.03570350349,1.16736750597208),.UNSPECIFIED.);
#173=B_SPLINE_CURVE_WITH_KNOTS('',3,(#7098,#7099,#7100,#7101,#7102,#7103,
#7104,#7105,#7106,#7107,#7108,#7109,#7110,#7111,#7112,#7113,#7114,#7115,
#7116,#7117,#7118,#7119),.UNSPECIFIED.,.F.,.F.,(4,2,2,2,2,2,2,2,2,2,4),
(0.0789094028588958,0.210573405340968,0.315860108011452,0.421146810681936,
0.522142632548711,0.623138454415486,0.72413427628226,0.825130098149035,
0.930416800819519,1.03570350349,1.16736750597208),.UNSPECIFIED.);
#174=B_SPLINE_CURVE_WITH_KNOTS('',3,(#7127,#7128,#7129,#7130,#7131,#7132,
#7133,#7134,#7135,#7136,#7137,#7138,#7139,#7140,#7141,#7142,#7143,#7144,
#7145,#7146,#7147,#7148),.UNSPECIFIED.,.F.,.F.,(4,2,2,2,2,2,2,2,2,2,4),
(0.0789094028588957,0.210573405340968,0.315860108011452,0.421146810681936,
0.522142632548711,0.623138454415485,0.72413427628226,0.825130098149035,
0.930416800819519,1.03570350349,1.16736750597207),.UNSPECIFIED.);
#175=B_SPLINE_CURVE_WITH_KNOTS('',3,(#7156,#7157,#7158,#7159,#7160,#7161,
#7162,#7163,#7164,#7165,#7166,#7167,#7168,#7169,#7170,#7171,#7172,#7173,
#7174,#7175,#7176,#7177),.UNSPECIFIED.,.F.,.F.,(4,2,2,2,2,2,2,2,2,2,4),
(0.0789094028588958,0.210573405340968,0.315860108011452,0.421146810681936,
0.522142632548711,0.623138454415486,0.72413427628226,0.825130098149035,
0.930416800819519,1.03570350349,1.16736750597208),.UNSPECIFIED.);
#176=B_SPLINE_CURVE_WITH_KNOTS('',3,(#7186,#7187,#7188,#7189,#7190,#7191,
#7192,#7193,#7194,#7195,#7196,#7197,#7198,#7199,#7200,#7201,#7202,#7203,
#7204,#7205,#7206,#7207),.UNSPECIFIED.,.F.,.F.,(4,2,2,2,2,2,2,2,2,2,4),
(0.0789094028588958,0.210573405340968,0.315860108011452,0.421146810681936,
0.522142632548711,0.623138454415485,0.72413427628226,0.825130098149035,
0.930416800819519,1.03570350349,1.16736750597208),.UNSPECIFIED.);
#177=B_SPLINE_CURVE_WITH_KNOTS('',3,(#7483,#7484,#7485,#7486,#7487,#7488,
#7489,#7490,#7491,#7492,#7493,#7494,#7495,#7496),.UNSPECIFIED.,.F.,.F.,
(4,2,2,2,2,2,4),(0.756005737987012,0.793568827564648,0.872922520054202,
0.952276212543757,1.03162990503331,1.11098359752287,1.1485466871005),
 .UNSPECIFIED.);
#178=B_SPLINE_CURVE_WITH_KNOTS('',3,(#7502,#7503,#7504,#7505,#7506,#7507,
#7508,#7509,#7510,#7511,#7512,#7513,#7514,#7515,#7516,#7517,#7518,#7519),
 .UNSPECIFIED.,.F.,.F.,(4,2,2,2,2,2,2,2,4),(0.,0.0792165807733632,0.158433161546726,
0.237648697074571,0.316864232602415,0.396079768130259,0.475295303658103,
0.554511884431466,0.63372846520483),.UNSPECIFIED.);
#179=B_SPLINE_CURVE_WITH_KNOTS('',3,(#7520,#7521,#7522,#7523,#7524,#7525,
#7526,#7527,#7528,#7529,#7530,#7531,#7532,#7533,#7534,#7535,#7536,#7537),
 .UNSPECIFIED.,.F.,.F.,(4,2,2,2,2,2,2,2,4),(0.63372846520483,0.712945045978192,
0.792161626751555,0.8713771622794,0.950592697807244,1.02980823333509,1.10902376886293,
1.1882403496363,1.26745693040966),.UNSPECIFIED.);
#180=B_SPLINE_CURVE_WITH_KNOTS('',3,(#7540,#7541,#7542,#7543,#7544,#7545,
#7546,#7547,#7548,#7549,#7550,#7551,#7552,#7553),.UNSPECIFIED.,.F.,.F.,
(4,2,2,2,2,2,4),(0.121154929624506,0.158718019202143,0.238071711691698,
0.317425404181252,0.396779096670807,0.476132789160362,0.513695878737999),
 .UNSPECIFIED.);
#181=B_SPLINE_CURVE_WITH_KNOTS('',3,(#7578,#7579,#7580,#7581,#7582,#7583,
#7584,#7585,#7586,#7587),.UNSPECIFIED.,.F.,.F.,(4,2,2,2,4),(0.803821788694075,
0.872950991853619,0.952307212900969,1.03166343394832,1.10079263710786),
 .UNSPECIFIED.);
#182=B_SPLINE_CURVE_WITH_KNOTS('',3,(#7593,#7594,#7595,#7596,#7597,#7598,
#7599,#7600,#7601,#7602,#7603,#7604,#7605,#7606,#7607,#7608,#7609,#7610),
 .UNSPECIFIED.,.F.,.F.,(4,2,2,2,2,2,2,2,4),(0.,0.0792028026112439,0.158405605222488,
0.237607602356377,0.316809599490266,0.396011596624156,0.475213593758045,
0.554416396369289,0.633619198980533),.UNSPECIFIED.);
#183=B_SPLINE_CURVE_WITH_KNOTS('',3,(#7611,#7612,#7613,#7614,#7615,#7616,
#7617,#7618,#7619,#7620,#7621,#7622,#7623,#7624,#7625,#7626,#7627,#7628),
 .UNSPECIFIED.,.F.,.F.,(4,2,2,2,2,2,2,2,4),(0.633619198980533,0.712822001591777,
0.792024804203021,0.87122680133691,0.9504287984708,1.02963079560469,1.10883279273858,
1.18803559534982,1.26723839796107),.UNSPECIFIED.);
#184=B_SPLINE_CURVE_WITH_KNOTS('',3,(#7631,#7632,#7633,#7634,#7635,#7636,
#7637,#7638,#7639,#7640),.UNSPECIFIED.,.F.,.F.,(4,2,2,2,4),(0.168950313426762,
0.238079516586307,0.317435737633656,0.396791958681006,0.465921161840551),
 .UNSPECIFIED.);
#185=SPHERICAL_SURFACE('',#4597,0.3969);
#186=SPHERICAL_SURFACE('',#4599,0.3969);
#187=SPHERICAL_SURFACE('',#4601,0.3969);
#188=SPHERICAL_SURFACE('',#4603,0.3969);
#189=SPHERICAL_SURFACE('',#4605,0.3969);
#190=SPHERICAL_SURFACE('',#4607,0.3969);
#191=SPHERICAL_SURFACE('',#4609,0.3969);
#192=SPHERICAL_SURFACE('',#4611,0.3969);
#193=SPHERICAL_SURFACE('',#4614,0.412776);
#194=SPHERICAL_SURFACE('',#4630,0.412776);
#195=SPHERICAL_SURFACE('',#4635,0.412776);
#196=SPHERICAL_SURFACE('',#4640,0.412776);
#197=SPHERICAL_SURFACE('',#4645,0.412776);
#198=SPHERICAL_SURFACE('',#4650,0.412776);
#199=SPHERICAL_SURFACE('',#4655,0.412776);
#200=SPHERICAL_SURFACE('',#4663,0.412776);
#201=CONICAL_SURFACE('',#4568,1.05,0.785398163397449);
#202=CONICAL_SURFACE('',#4575,1.05,0.785398163397449);
#203=CONICAL_SURFACE('',#4588,2.3,0.785398163397449);
#204=CONICAL_SURFACE('',#4592,2.3,0.785398163397449);
#205=CONICAL_SURFACE('',#4692,0.475,0.785398163397449);
#206=CONICAL_SURFACE('',#4696,0.485,0.785398163397448);
#207=CONICAL_SURFACE('',#4700,0.31,0.463647609000806);
#208=CONICAL_SURFACE('',#4704,0.27,0.785398163397448);
#209=CONICAL_SURFACE('',#4718,0.325,0.785398163397448);
#210=CONICAL_SURFACE('',#4722,0.335,0.785398163397448);
#211=CONICAL_SURFACE('',#4726,0.21,0.463647609000806);
#212=CONICAL_SURFACE('',#4730,0.18,0.785398163397448);
#213=CONICAL_SURFACE('',#4864,0.235,0.785398163397448);
#214=CONICAL_SURFACE('',#4868,0.2125,0.785398163397448);
#215=TOROIDAL_SURFACE('',#4557,1.675,0.412776);
#216=TOROIDAL_SURFACE('',#4577,1.675,0.412776);
#217=SHAPE_REPRESENTATION_RELATIONSHIP('SRR','None',#7964,#238);
#218=SHAPE_REPRESENTATION_RELATIONSHIP('SRR','None',#7965,#239);
#219=SHAPE_REPRESENTATION_RELATIONSHIP('SRR','None',#7966,#240);
#220=SHAPE_REPRESENTATION_RELATIONSHIP('SRR','None',#7967,#241);
#221=SHAPE_REPRESENTATION_RELATIONSHIP('SRR','None',#7968,#242);
#222=SHAPE_REPRESENTATION_RELATIONSHIP('SRR','None',#7969,#243);
#223=SHAPE_REPRESENTATION_RELATIONSHIP('SRR','None',#7970,#244);
#224=SHAPE_REPRESENTATION_RELATIONSHIP('SRR','None',#7971,#245);
#225=SHAPE_REPRESENTATION_RELATIONSHIP('SRR','None',#7973,#246);
#226=SHAPE_REPRESENTATION_RELATIONSHIP('SRR','None',#7974,#247);
#227=SHAPE_REPRESENTATION_RELATIONSHIP('SRR','None',#7975,#248);
#228=SHAPE_REPRESENTATION_RELATIONSHIP('SRR','None',#7976,#249);
#229=SHAPE_REPRESENTATION_RELATIONSHIP('SRR','None',#7977,#250);
#230=SHAPE_REPRESENTATION_RELATIONSHIP('SRR','None',#7978,#251);
#231=SHAPE_REPRESENTATION_RELATIONSHIP('SRR','None',#7979,#252);
#232=SHAPE_REPRESENTATION_RELATIONSHIP('SRR','None',#7981,#253);
#233=SHAPE_REPRESENTATION_RELATIONSHIP('SRR','None',#7982,#254);
#234=SHAPE_REPRESENTATION_RELATIONSHIP('SRR','None',#7983,#255);
#235=SHAPE_REPRESENTATION_RELATIONSHIP('SRR','None',#7984,#256);
#236=SHAPE_REPRESENTATION_RELATIONSHIP('SRR','None',#7985,#257);
#237=SHAPE_REPRESENTATION_RELATIONSHIP('SRR','None',#7986,#258);
#238=ADVANCED_BREP_SHAPE_REPRESENTATION('',(#288),#7848);
#239=ADVANCED_BREP_SHAPE_REPRESENTATION('',(#289),#7849);
#240=ADVANCED_BREP_SHAPE_REPRESENTATION('',(#290),#7850);
#241=ADVANCED_BREP_SHAPE_REPRESENTATION('',(#291),#7851);
#242=ADVANCED_BREP_SHAPE_REPRESENTATION('',(#292),#7852);
#243=ADVANCED_BREP_SHAPE_REPRESENTATION('',(#293),#7853);
#244=ADVANCED_BREP_SHAPE_REPRESENTATION('',(#294),#7854);
#245=ADVANCED_BREP_SHAPE_REPRESENTATION('',(#295),#7855);
#246=ADVANCED_BREP_SHAPE_REPRESENTATION('',(#296),#7857);
#247=ADVANCED_BREP_SHAPE_REPRESENTATION('',(#297),#7858);
#248=ADVANCED_BREP_SHAPE_REPRESENTATION('',(#298,#299,#300,#301,#302,#303,
#304,#305),#7859);
#249=ADVANCED_BREP_SHAPE_REPRESENTATION('',(#306),#7860);
#250=ADVANCED_BREP_SHAPE_REPRESENTATION('',(#307,#308),#7861);
#251=ADVANCED_BREP_SHAPE_REPRESENTATION('',(#13),#7862);
#252=ADVANCED_BREP_SHAPE_REPRESENTATION('',(#14),#7863);
#253=ADVANCED_BREP_SHAPE_REPRESENTATION('',(#309),#7865);
#254=ADVANCED_BREP_SHAPE_REPRESENTATION('',(#310),#7866);
#255=ADVANCED_BREP_SHAPE_REPRESENTATION('',(#311),#7867);
#256=ADVANCED_BREP_SHAPE_REPRESENTATION('',(#312),#7868);
#257=ADVANCED_BREP_SHAPE_REPRESENTATION('',(#313),#7869);
#258=ADVANCED_BREP_SHAPE_REPRESENTATION('',(#314),#7870);
#259=STYLED_ITEM('',(#8132),#288);
#260=STYLED_ITEM('',(#8132),#289);
#261=STYLED_ITEM('',(#8153),#290);
#262=STYLED_ITEM('',(#8160),#291);
#263=STYLED_ITEM('',(#8160),#292);
#264=STYLED_ITEM('',(#8146),#293);
#265=STYLED_ITEM('',(#8132),#294);
#266=STYLED_ITEM('',(#8132),#295);
#267=STYLED_ITEM('',(#8153),#296);
#268=STYLED_ITEM('',(#8153),#297);
#269=STYLED_ITEM('',(#8153),#298);
#270=STYLED_ITEM('',(#8153),#299);
#271=STYLED_ITEM('',(#8153),#300);
#272=STYLED_ITEM('',(#8153),#301);
#273=STYLED_ITEM('',(#8153),#302);
#274=STYLED_ITEM('',(#8153),#303);
#275=STYLED_ITEM('',(#8153),#304);
#276=STYLED_ITEM('',(#8153),#305);
#277=STYLED_ITEM('',(#8153),#306);
#278=STYLED_ITEM('',(#8153),#307);
#279=STYLED_ITEM('',(#8153),#308);
#280=STYLED_ITEM('',(#8160),#13);
#281=STYLED_ITEM('',(#8160),#14);
#282=STYLED_ITEM('',(#8153),#309);
#283=STYLED_ITEM('',(#8153),#310);
#284=STYLED_ITEM('',(#8153),#311);
#285=STYLED_ITEM('',(#8146),#312);
#286=STYLED_ITEM('',(#8153),#313);
#287=STYLED_ITEM('',(#8160),#314);
#288=MANIFOLD_SOLID_BREP('Body1',#4085);
#289=MANIFOLD_SOLID_BREP('Body1',#4086);
#290=MANIFOLD_SOLID_BREP('Body1',#4087);
#291=MANIFOLD_SOLID_BREP('Body1',#4088);
#292=MANIFOLD_SOLID_BREP('Body1',#4089);
#293=MANIFOLD_SOLID_BREP('Body1',#4090);
#294=MANIFOLD_SOLID_BREP('Body1',#4091);
#295=MANIFOLD_SOLID_BREP('Body1',#4092);
#296=MANIFOLD_SOLID_BREP('Body1',#4093);
#297=MANIFOLD_SOLID_BREP('Body1',#4094);
#298=MANIFOLD_SOLID_BREP('Body1',#4095);
#299=MANIFOLD_SOLID_BREP('Body2',#4096);
#300=MANIFOLD_SOLID_BREP('Body3',#4097);
#301=MANIFOLD_SOLID_BREP('Body4',#4098);
#302=MANIFOLD_SOLID_BREP('Body5',#4099);
#303=MANIFOLD_SOLID_BREP('Body6',#4100);
#304=MANIFOLD_SOLID_BREP('Body7',#4101);
#305=MANIFOLD_SOLID_BREP('Body8',#4102);
#306=MANIFOLD_SOLID_BREP('Continuous crown cage',#4103);
#307=MANIFOLD_SOLID_BREP('Body1',#4104);
#308=MANIFOLD_SOLID_BREP('Body2',#4105);
#309=MANIFOLD_SOLID_BREP('Body1',#4110);
#310=MANIFOLD_SOLID_BREP('Body1',#4111);
#311=MANIFOLD_SOLID_BREP('Body1',#4112);
#312=MANIFOLD_SOLID_BREP('Body1',#4113);
#313=MANIFOLD_SOLID_BREP('Body1',#4114);
#314=MANIFOLD_SOLID_BREP('Body1',#4115);
#315=FACE_BOUND('',#812,.T.);
#316=FACE_BOUND('',#813,.T.);
#317=FACE_BOUND('',#814,.T.);
#318=FACE_BOUND('',#815,.T.);
#319=FACE_BOUND('',#817,.T.);
#320=FACE_BOUND('',#818,.T.);
#321=FACE_BOUND('',#819,.T.);
#322=FACE_BOUND('',#820,.T.);
#323=FACE_BOUND('',#846,.T.);
#324=FACE_BOUND('',#848,.T.);
#325=FACE_BOUND('',#851,.T.);
#326=FACE_BOUND('',#852,.T.);
#327=FACE_BOUND('',#859,.T.);
#328=FACE_BOUND('',#861,.T.);
#329=FACE_BOUND('',#864,.T.);
#330=FACE_BOUND('',#865,.T.);
#331=FACE_BOUND('',#869,.T.);
#332=FACE_BOUND('',#870,.T.);
#333=FACE_BOUND('',#872,.T.);
#334=FACE_BOUND('',#873,.T.);
#335=FACE_BOUND('',#874,.T.);
#336=FACE_BOUND('',#875,.T.);
#337=FACE_BOUND('',#876,.T.);
#338=FACE_BOUND('',#878,.T.);
#339=FACE_BOUND('',#879,.T.);
#340=FACE_BOUND('',#880,.T.);
#341=FACE_BOUND('',#881,.T.);
#342=FACE_BOUND('',#882,.T.);
#343=FACE_BOUND('',#886,.T.);
#344=FACE_BOUND('',#888,.T.);
#345=FACE_BOUND('',#895,.T.);
#346=FACE_BOUND('',#898,.T.);
#347=FACE_BOUND('',#902,.T.);
#348=FACE_BOUND('',#903,.T.);
#349=FACE_BOUND('',#904,.T.);
#350=FACE_BOUND('',#905,.T.);
#351=FACE_BOUND('',#906,.T.);
#352=FACE_BOUND('',#908,.T.);
#353=FACE_BOUND('',#909,.T.);
#354=FACE_BOUND('',#910,.T.);
#355=FACE_BOUND('',#911,.T.);
#356=FACE_BOUND('',#912,.T.);
#357=FACE_BOUND('',#916,.T.);
#358=FACE_BOUND('',#918,.T.);
#359=FACE_BOUND('',#921,.T.);
#360=FACE_BOUND('',#924,.T.);
#361=FACE_BOUND('',#927,.T.);
#362=FACE_BOUND('',#930,.T.);
#363=FACE_BOUND('',#936,.T.);
#364=FACE_BOUND('',#940,.T.);
#365=FACE_BOUND('',#945,.T.);
#366=FACE_BOUND('',#946,.T.);
#367=FACE_BOUND('',#947,.T.);
#368=FACE_BOUND('',#948,.T.);
#369=FACE_BOUND('',#950,.T.);
#370=FACE_BOUND('',#951,.T.);
#371=FACE_BOUND('',#952,.T.);
#372=FACE_BOUND('',#953,.T.);
#373=FACE_BOUND('',#954,.T.);
#374=FACE_BOUND('',#972,.T.);
#375=FACE_BOUND('',#975,.T.);
#376=FACE_BOUND('',#980,.T.);
#377=FACE_BOUND('',#985,.T.);
#378=FACE_BOUND('',#1013,.T.);
#379=FACE_BOUND('',#1016,.T.);
#380=FACE_BOUND('',#1019,.T.);
#381=FACE_BOUND('',#1022,.T.);
#382=FACE_BOUND('',#1025,.T.);
#383=FACE_BOUND('',#1032,.T.);
#384=FACE_BOUND('',#1050,.T.);
#385=FACE_BOUND('',#1069,.T.);
#386=FACE_BOUND('',#1071,.T.);
#387=FACE_BOUND('',#1074,.T.);
#388=FACE_BOUND('',#1081,.T.);
#389=FACE_BOUND('',#1083,.T.);
#390=FACE_BOUND('',#1088,.T.);
#391=FACE_BOUND('',#1090,.T.);
#392=FACE_BOUND('',#1092,.T.);
#393=FACE_BOUND('',#1094,.T.);
#394=FACE_BOUND('',#1102,.T.);
#395=FACE_BOUND('',#1104,.T.);
#396=FACE_BOUND('',#1110,.T.);
#397=FACE_BOUND('',#1111,.T.);
#398=FACE_BOUND('',#1112,.T.);
#399=FACE_BOUND('',#1113,.T.);
#400=FACE_BOUND('',#1114,.T.);
#401=FACE_BOUND('',#1117,.T.);
#402=FACE_BOUND('',#1119,.T.);
#403=FACE_BOUND('',#1120,.T.);
#404=FACE_BOUND('',#1121,.T.);
#405=FACE_BOUND('',#1122,.T.);
#406=FACE_BOUND('',#1123,.T.);
#407=FACE_BOUND('',#1142,.T.);
#408=PLANE('',#4363);
#409=PLANE('',#4364);
#410=PLANE('',#4365);
#411=PLANE('',#4366);
#412=PLANE('',#4367);
#413=PLANE('',#4368);
#414=PLANE('',#4373);
#415=PLANE('',#4377);
#416=PLANE('',#4381);
#417=PLANE('',#4385);
#418=PLANE('',#4389);
#419=PLANE('',#4393);
#420=PLANE('',#4397);
#421=PLANE('',#4401);
#422=PLANE('',#4414);
#423=PLANE('',#4416);
#424=PLANE('',#4418);
#425=PLANE('',#4420);
#426=PLANE('',#4422);
#427=PLANE('',#4423);
#428=PLANE('',#4424);
#429=PLANE('',#4425);
#430=PLANE('',#4426);
#431=PLANE('',#4427);
#432=PLANE('',#4429);
#433=PLANE('',#4431);
#434=PLANE('',#4433);
#435=PLANE('',#4435);
#436=PLANE('',#4436);
#437=PLANE('',#4437);
#438=PLANE('',#4438);
#439=PLANE('',#4439);
#440=PLANE('',#4446);
#441=PLANE('',#4447);
#442=PLANE('',#4455);
#443=PLANE('',#4456);
#444=PLANE('',#4473);
#445=PLANE('',#4478);
#446=PLANE('',#4484);
#447=PLANE('',#4485);
#448=PLANE('',#4493);
#449=PLANE('',#4494);
#450=PLANE('',#4499);
#451=PLANE('',#4504);
#452=PLANE('',#4509);
#453=PLANE('',#4514);
#454=PLANE('',#4524);
#455=PLANE('',#4532);
#456=PLANE('',#4535);
#457=PLANE('',#4539);
#458=PLANE('',#4540);
#459=PLANE('',#4542);
#460=PLANE('',#4543);
#461=PLANE('',#4544);
#462=PLANE('',#4545);
#463=PLANE('',#4546);
#464=PLANE('',#4547);
#465=PLANE('',#4549);
#466=PLANE('',#4550);
#467=PLANE('',#4551);
#468=PLANE('',#4552);
#469=PLANE('',#4553);
#470=PLANE('',#4554);
#471=PLANE('',#4570);
#472=PLANE('',#4573);
#473=PLANE('',#4585);
#474=PLANE('',#4594);
#475=PLANE('',#4627);
#476=PLANE('',#4632);
#477=PLANE('',#4637);
#478=PLANE('',#4642);
#479=PLANE('',#4647);
#480=PLANE('',#4652);
#481=PLANE('',#4661);
#482=PLANE('',#4665);
#483=PLANE('',#4666);
#484=PLANE('',#4668);
#485=PLANE('',#4673);
#486=PLANE('',#4676);
#487=PLANE('',#4681);
#488=PLANE('',#4690);
#489=PLANE('',#4698);
#490=PLANE('',#4706);
#491=PLANE('',#4707);
#492=PLANE('',#4708);
#493=PLANE('',#4709);
#494=PLANE('',#4710);
#495=PLANE('',#4711);
#496=PLANE('',#4712);
#497=PLANE('',#4713);
#498=PLANE('',#4714);
#499=PLANE('',#4716);
#500=PLANE('',#4724);
#501=PLANE('',#4732);
#502=PLANE('',#4733);
#503=PLANE('',#4734);
#504=PLANE('',#4735);
#505=PLANE('',#4736);
#506=PLANE('',#4737);
#507=PLANE('',#4738);
#508=PLANE('',#4739);
#509=PLANE('',#4740);
#510=PLANE('',#4765);
#511=PLANE('',#4766);
#512=PLANE('',#4768);
#513=PLANE('',#4769);
#514=PLANE('',#4770);
#515=PLANE('',#4772);
#516=PLANE('',#4775);
#517=PLANE('',#4783);
#518=PLANE('',#4784);
#519=PLANE('',#4792);
#520=PLANE('',#4793);
#521=PLANE('',#4795);
#522=PLANE('',#4800);
#523=PLANE('',#4807);
#524=PLANE('',#4808);
#525=PLANE('',#4810);
#526=PLANE('',#4815);
#527=PLANE('',#4816);
#528=PLANE('',#4817);
#529=PLANE('',#4818);
#530=PLANE('',#4819);
#531=PLANE('',#4836);
#532=PLANE('',#4842);
#533=PLANE('',#4844);
#534=PLANE('',#4845);
#535=PLANE('',#4846);
#536=PLANE('',#4847);
#537=PLANE('',#4848);
#538=PLANE('',#4849);
#539=PLANE('',#4850);
#540=PLANE('',#4851);
#541=PLANE('',#4852);
#542=PLANE('',#4853);
#543=PLANE('',#4855);
#544=PLANE('',#4856);
#545=PLANE('',#4857);
#546=PLANE('',#4858);
#547=PLANE('',#4859);
#548=PLANE('',#4860);
#549=PLANE('',#4861);
#550=PLANE('',#4862);
#551=PLANE('',#4870);
#552=FACE_OUTER_BOUND('',#803,.T.);
#553=FACE_OUTER_BOUND('',#804,.T.);
#554=FACE_OUTER_BOUND('',#805,.T.);
#555=FACE_OUTER_BOUND('',#806,.T.);
#556=FACE_OUTER_BOUND('',#807,.T.);
#557=FACE_OUTER_BOUND('',#808,.T.);
#558=FACE_OUTER_BOUND('',#809,.T.);
#559=FACE_OUTER_BOUND('',#810,.T.);
#560=FACE_OUTER_BOUND('',#811,.T.);
#561=FACE_OUTER_BOUND('',#816,.T.);
#562=FACE_OUTER_BOUND('',#821,.T.);
#563=FACE_OUTER_BOUND('',#822,.T.);
#564=FACE_OUTER_BOUND('',#823,.T.);
#565=FACE_OUTER_BOUND('',#824,.T.);
#566=FACE_OUTER_BOUND('',#825,.T.);
#567=FACE_OUTER_BOUND('',#826,.T.);
#568=FACE_OUTER_BOUND('',#827,.T.);
#569=FACE_OUTER_BOUND('',#828,.T.);
#570=FACE_OUTER_BOUND('',#829,.T.);
#571=FACE_OUTER_BOUND('',#830,.T.);
#572=FACE_OUTER_BOUND('',#831,.T.);
#573=FACE_OUTER_BOUND('',#832,.T.);
#574=FACE_OUTER_BOUND('',#833,.T.);
#575=FACE_OUTER_BOUND('',#834,.T.);
#576=FACE_OUTER_BOUND('',#835,.T.);
#577=FACE_OUTER_BOUND('',#836,.T.);
#578=FACE_OUTER_BOUND('',#837,.T.);
#579=FACE_OUTER_BOUND('',#838,.T.);
#580=FACE_OUTER_BOUND('',#839,.T.);
#581=FACE_OUTER_BOUND('',#840,.T.);
#582=FACE_OUTER_BOUND('',#841,.T.);
#583=FACE_OUTER_BOUND('',#842,.T.);
#584=FACE_OUTER_BOUND('',#843,.T.);
#585=FACE_OUTER_BOUND('',#844,.T.);
#586=FACE_OUTER_BOUND('',#845,.T.);
#587=FACE_OUTER_BOUND('',#847,.T.);
#588=FACE_OUTER_BOUND('',#849,.T.);
#589=FACE_OUTER_BOUND('',#850,.T.);
#590=FACE_OUTER_BOUND('',#853,.T.);
#591=FACE_OUTER_BOUND('',#854,.T.);
#592=FACE_OUTER_BOUND('',#855,.T.);
#593=FACE_OUTER_BOUND('',#856,.T.);
#594=FACE_OUTER_BOUND('',#857,.T.);
#595=FACE_OUTER_BOUND('',#858,.T.);
#596=FACE_OUTER_BOUND('',#860,.T.);
#597=FACE_OUTER_BOUND('',#862,.T.);
#598=FACE_OUTER_BOUND('',#863,.T.);
#599=FACE_OUTER_BOUND('',#866,.T.);
#600=FACE_OUTER_BOUND('',#867,.T.);
#601=FACE_OUTER_BOUND('',#868,.T.);
#602=FACE_OUTER_BOUND('',#871,.T.);
#603=FACE_OUTER_BOUND('',#877,.T.);
#604=FACE_OUTER_BOUND('',#883,.T.);
#605=FACE_OUTER_BOUND('',#884,.T.);
#606=FACE_OUTER_BOUND('',#885,.T.);
#607=FACE_OUTER_BOUND('',#887,.T.);
#608=FACE_OUTER_BOUND('',#889,.T.);
#609=FACE_OUTER_BOUND('',#890,.T.);
#610=FACE_OUTER_BOUND('',#891,.T.);
#611=FACE_OUTER_BOUND('',#892,.T.);
#612=FACE_OUTER_BOUND('',#893,.T.);
#613=FACE_OUTER_BOUND('',#894,.T.);
#614=FACE_OUTER_BOUND('',#896,.T.);
#615=FACE_OUTER_BOUND('',#897,.T.);
#616=FACE_OUTER_BOUND('',#899,.T.);
#617=FACE_OUTER_BOUND('',#900,.T.);
#618=FACE_OUTER_BOUND('',#901,.T.);
#619=FACE_OUTER_BOUND('',#907,.T.);
#620=FACE_OUTER_BOUND('',#913,.T.);
#621=FACE_OUTER_BOUND('',#914,.T.);
#622=FACE_OUTER_BOUND('',#915,.T.);
#623=FACE_OUTER_BOUND('',#917,.T.);
#624=FACE_OUTER_BOUND('',#919,.T.);
#625=FACE_OUTER_BOUND('',#920,.T.);
#626=FACE_OUTER_BOUND('',#922,.T.);
#627=FACE_OUTER_BOUND('',#923,.T.);
#628=FACE_OUTER_BOUND('',#925,.T.);
#629=FACE_OUTER_BOUND('',#926,.T.);
#630=FACE_OUTER_BOUND('',#928,.T.);
#631=FACE_OUTER_BOUND('',#929,.T.);
#632=FACE_OUTER_BOUND('',#931,.T.);
#633=FACE_OUTER_BOUND('',#932,.T.);
#634=FACE_OUTER_BOUND('',#933,.T.);
#635=FACE_OUTER_BOUND('',#934,.T.);
#636=FACE_OUTER_BOUND('',#935,.T.);
#637=FACE_OUTER_BOUND('',#937,.T.);
#638=FACE_OUTER_BOUND('',#938,.T.);
#639=FACE_OUTER_BOUND('',#939,.T.);
#640=FACE_OUTER_BOUND('',#941,.T.);
#641=FACE_OUTER_BOUND('',#942,.T.);
#642=FACE_OUTER_BOUND('',#943,.T.);
#643=FACE_OUTER_BOUND('',#944,.T.);
#644=FACE_OUTER_BOUND('',#949,.T.);
#645=FACE_OUTER_BOUND('',#955,.T.);
#646=FACE_OUTER_BOUND('',#956,.T.);
#647=FACE_OUTER_BOUND('',#957,.T.);
#648=FACE_OUTER_BOUND('',#958,.T.);
#649=FACE_OUTER_BOUND('',#959,.T.);
#650=FACE_OUTER_BOUND('',#960,.T.);
#651=FACE_OUTER_BOUND('',#961,.T.);
#652=FACE_OUTER_BOUND('',#962,.T.);
#653=FACE_OUTER_BOUND('',#963,.T.);
#654=FACE_OUTER_BOUND('',#964,.T.);
#655=FACE_OUTER_BOUND('',#965,.T.);
#656=FACE_OUTER_BOUND('',#966,.T.);
#657=FACE_OUTER_BOUND('',#967,.T.);
#658=FACE_OUTER_BOUND('',#968,.T.);
#659=FACE_OUTER_BOUND('',#969,.T.);
#660=FACE_OUTER_BOUND('',#970,.T.);
#661=FACE_OUTER_BOUND('',#971,.T.);
#662=FACE_OUTER_BOUND('',#973,.T.);
#663=FACE_OUTER_BOUND('',#974,.T.);
#664=FACE_OUTER_BOUND('',#976,.T.);
#665=FACE_OUTER_BOUND('',#977,.T.);
#666=FACE_OUTER_BOUND('',#978,.T.);
#667=FACE_OUTER_BOUND('',#979,.T.);
#668=FACE_OUTER_BOUND('',#981,.T.);
#669=FACE_OUTER_BOUND('',#982,.T.);
#670=FACE_OUTER_BOUND('',#983,.T.);
#671=FACE_OUTER_BOUND('',#984,.T.);
#672=FACE_OUTER_BOUND('',#986,.T.);
#673=FACE_OUTER_BOUND('',#987,.T.);
#674=FACE_OUTER_BOUND('',#988,.T.);
#675=FACE_OUTER_BOUND('',#989,.T.);
#676=FACE_OUTER_BOUND('',#990,.T.);
#677=FACE_OUTER_BOUND('',#991,.T.);
#678=FACE_OUTER_BOUND('',#992,.T.);
#679=FACE_OUTER_BOUND('',#993,.T.);
#680=FACE_OUTER_BOUND('',#994,.T.);
#681=FACE_OUTER_BOUND('',#995,.T.);
#682=FACE_OUTER_BOUND('',#996,.T.);
#683=FACE_OUTER_BOUND('',#997,.T.);
#684=FACE_OUTER_BOUND('',#998,.T.);
#685=FACE_OUTER_BOUND('',#999,.T.);
#686=FACE_OUTER_BOUND('',#1000,.T.);
#687=FACE_OUTER_BOUND('',#1001,.T.);
#688=FACE_OUTER_BOUND('',#1002,.T.);
#689=FACE_OUTER_BOUND('',#1003,.T.);
#690=FACE_OUTER_BOUND('',#1004,.T.);
#691=FACE_OUTER_BOUND('',#1005,.T.);
#692=FACE_OUTER_BOUND('',#1006,.T.);
#693=FACE_OUTER_BOUND('',#1007,.T.);
#694=FACE_OUTER_BOUND('',#1008,.T.);
#695=FACE_OUTER_BOUND('',#1009,.T.);
#696=FACE_OUTER_BOUND('',#1010,.T.);
#697=FACE_OUTER_BOUND('',#1011,.T.);
#698=FACE_OUTER_BOUND('',#1012,.T.);
#699=FACE_OUTER_BOUND('',#1014,.T.);
#700=FACE_OUTER_BOUND('',#1015,.T.);
#701=FACE_OUTER_BOUND('',#1017,.T.);
#702=FACE_OUTER_BOUND('',#1018,.T.);
#703=FACE_OUTER_BOUND('',#1020,.T.);
#704=FACE_OUTER_BOUND('',#1021,.T.);
#705=FACE_OUTER_BOUND('',#1023,.T.);
#706=FACE_OUTER_BOUND('',#1024,.T.);
#707=FACE_OUTER_BOUND('',#1026,.T.);
#708=FACE_OUTER_BOUND('',#1027,.T.);
#709=FACE_OUTER_BOUND('',#1028,.T.);
#710=FACE_OUTER_BOUND('',#1029,.T.);
#711=FACE_OUTER_BOUND('',#1030,.T.);
#712=FACE_OUTER_BOUND('',#1031,.T.);
#713=FACE_OUTER_BOUND('',#1033,.T.);
#714=FACE_OUTER_BOUND('',#1034,.T.);
#715=FACE_OUTER_BOUND('',#1035,.T.);
#716=FACE_OUTER_BOUND('',#1036,.T.);
#717=FACE_OUTER_BOUND('',#1037,.T.);
#718=FACE_OUTER_BOUND('',#1038,.T.);
#719=FACE_OUTER_BOUND('',#1039,.T.);
#720=FACE_OUTER_BOUND('',#1040,.T.);
#721=FACE_OUTER_BOUND('',#1041,.T.);
#722=FACE_OUTER_BOUND('',#1042,.T.);
#723=FACE_OUTER_BOUND('',#1043,.T.);
#724=FACE_OUTER_BOUND('',#1044,.T.);
#725=FACE_OUTER_BOUND('',#1045,.T.);
#726=FACE_OUTER_BOUND('',#1046,.T.);
#727=FACE_OUTER_BOUND('',#1047,.T.);
#728=FACE_OUTER_BOUND('',#1048,.T.);
#729=FACE_OUTER_BOUND('',#1049,.T.);
#730=FACE_OUTER_BOUND('',#1051,.T.);
#731=FACE_OUTER_BOUND('',#1052,.T.);
#732=FACE_OUTER_BOUND('',#1053,.T.);
#733=FACE_OUTER_BOUND('',#1054,.T.);
#734=FACE_OUTER_BOUND('',#1055,.T.);
#735=FACE_OUTER_BOUND('',#1056,.T.);
#736=FACE_OUTER_BOUND('',#1057,.T.);
#737=FACE_OUTER_BOUND('',#1058,.T.);
#738=FACE_OUTER_BOUND('',#1059,.T.);
#739=FACE_OUTER_BOUND('',#1060,.T.);
#740=FACE_OUTER_BOUND('',#1061,.T.);
#741=FACE_OUTER_BOUND('',#1062,.T.);
#742=FACE_OUTER_BOUND('',#1063,.T.);
#743=FACE_OUTER_BOUND('',#1064,.T.);
#744=FACE_OUTER_BOUND('',#1065,.T.);
#745=FACE_OUTER_BOUND('',#1066,.T.);
#746=FACE_OUTER_BOUND('',#1067,.T.);
#747=FACE_OUTER_BOUND('',#1068,.T.);
#748=FACE_OUTER_BOUND('',#1070,.T.);
#749=FACE_OUTER_BOUND('',#1072,.T.);
#750=FACE_OUTER_BOUND('',#1073,.T.);
#751=FACE_OUTER_BOUND('',#1075,.T.);
#752=FACE_OUTER_BOUND('',#1076,.T.);
#753=FACE_OUTER_BOUND('',#1077,.T.);
#754=FACE_OUTER_BOUND('',#1078,.T.);
#755=FACE_OUTER_BOUND('',#1079,.T.);
#756=FACE_OUTER_BOUND('',#1080,.T.);
#757=FACE_OUTER_BOUND('',#1082,.T.);
#758=FACE_OUTER_BOUND('',#1084,.T.);
#759=FACE_OUTER_BOUND('',#1085,.T.);
#760=FACE_OUTER_BOUND('',#1086,.T.);
#761=FACE_OUTER_BOUND('',#1087,.T.);
#762=FACE_OUTER_BOUND('',#1089,.T.);
#763=FACE_OUTER_BOUND('',#1091,.T.);
#764=FACE_OUTER_BOUND('',#1093,.T.);
#765=FACE_OUTER_BOUND('',#1095,.T.);
#766=FACE_OUTER_BOUND('',#1096,.T.);
#767=FACE_OUTER_BOUND('',#1097,.T.);
#768=FACE_OUTER_BOUND('',#1098,.T.);
#769=FACE_OUTER_BOUND('',#1099,.T.);
#770=FACE_OUTER_BOUND('',#1100,.T.);
#771=FACE_OUTER_BOUND('',#1101,.T.);
#772=FACE_OUTER_BOUND('',#1103,.T.);
#773=FACE_OUTER_BOUND('',#1105,.T.);
#774=FACE_OUTER_BOUND('',#1106,.T.);
#775=FACE_OUTER_BOUND('',#1107,.T.);
#776=FACE_OUTER_BOUND('',#1108,.T.);
#777=FACE_OUTER_BOUND('',#1109,.T.);
#778=FACE_OUTER_BOUND('',#1115,.T.);
#779=FACE_OUTER_BOUND('',#1116,.T.);
#780=FACE_OUTER_BOUND('',#1118,.T.);
#781=FACE_OUTER_BOUND('',#1124,.T.);
#782=FACE_OUTER_BOUND('',#1125,.T.);
#783=FACE_OUTER_BOUND('',#1126,.T.);
#784=FACE_OUTER_BOUND('',#1127,.T.);
#785=FACE_OUTER_BOUND('',#1128,.T.);
#786=FACE_OUTER_BOUND('',#1129,.T.);
#787=FACE_OUTER_BOUND('',#1130,.T.);
#788=FACE_OUTER_BOUND('',#1131,.T.);
#789=FACE_OUTER_BOUND('',#1132,.T.);
#790=FACE_OUTER_BOUND('',#1133,.T.);
#791=FACE_OUTER_BOUND('',#1134,.T.);
#792=FACE_OUTER_BOUND('',#1135,.T.);
#793=FACE_OUTER_BOUND('',#1136,.T.);
#794=FACE_OUTER_BOUND('',#1137,.T.);
#795=FACE_OUTER_BOUND('',#1138,.T.);
#796=FACE_OUTER_BOUND('',#1139,.T.);
#797=FACE_OUTER_BOUND('',#1140,.T.);
#798=FACE_OUTER_BOUND('',#1141,.T.);
#799=FACE_OUTER_BOUND('',#1143,.T.);
#800=FACE_OUTER_BOUND('',#1144,.T.);
#801=FACE_OUTER_BOUND('',#1145,.T.);
#802=FACE_OUTER_BOUND('',#1146,.T.);
#803=EDGE_LOOP('',(#2743,#2744,#2745,#2746));
#804=EDGE_LOOP('',(#2747,#2748,#2749,#2750));
#805=EDGE_LOOP('',(#2751,#2752,#2753,#2754));
#806=EDGE_LOOP('',(#2755,#2756,#2757,#2758));
#807=EDGE_LOOP('',(#2759,#2760,#2761,#2762));
#808=EDGE_LOOP('',(#2763,#2764,#2765,#2766));
#809=EDGE_LOOP('',(#2767,#2768,#2769,#2770));
#810=EDGE_LOOP('',(#2771,#2772,#2773,#2774));
#811=EDGE_LOOP('',(#2775,#2776,#2777,#2778));
#812=EDGE_LOOP('',(#2779));
#813=EDGE_LOOP('',(#2780));
#814=EDGE_LOOP('',(#2781));
#815=EDGE_LOOP('',(#2782));
#816=EDGE_LOOP('',(#2783,#2784,#2785,#2786));
#817=EDGE_LOOP('',(#2787));
#818=EDGE_LOOP('',(#2788));
#819=EDGE_LOOP('',(#2789));
#820=EDGE_LOOP('',(#2790));
#821=EDGE_LOOP('',(#2791,#2792,#2793,#2794));
#822=EDGE_LOOP('',(#2795));
#823=EDGE_LOOP('',(#2796,#2797,#2798,#2799));
#824=EDGE_LOOP('',(#2800));
#825=EDGE_LOOP('',(#2801,#2802,#2803,#2804));
#826=EDGE_LOOP('',(#2805));
#827=EDGE_LOOP('',(#2806,#2807,#2808,#2809));
#828=EDGE_LOOP('',(#2810));
#829=EDGE_LOOP('',(#2811,#2812,#2813,#2814));
#830=EDGE_LOOP('',(#2815));
#831=EDGE_LOOP('',(#2816,#2817,#2818,#2819));
#832=EDGE_LOOP('',(#2820));
#833=EDGE_LOOP('',(#2821,#2822,#2823,#2824));
#834=EDGE_LOOP('',(#2825));
#835=EDGE_LOOP('',(#2826,#2827,#2828,#2829));
#836=EDGE_LOOP('',(#2830));
#837=EDGE_LOOP('',(#2831,#2832,#2833,#2834));
#838=EDGE_LOOP('',(#2835,#2836,#2837,#2838));
#839=EDGE_LOOP('',(#2839,#2840,#2841,#2842));
#840=EDGE_LOOP('',(#2843,#2844,#2845,#2846));
#841=EDGE_LOOP('',(#2847,#2848,#2849,#2850));
#842=EDGE_LOOP('',(#2851,#2852,#2853,#2854));
#843=EDGE_LOOP('',(#2855,#2856,#2857,#2858));
#844=EDGE_LOOP('',(#2859,#2860,#2861,#2862));
#845=EDGE_LOOP('',(#2863,#2864,#2865,#2866));
#846=EDGE_LOOP('',(#2867));
#847=EDGE_LOOP('',(#2868,#2869,#2870,#2871));
#848=EDGE_LOOP('',(#2872));
#849=EDGE_LOOP('',(#2873,#2874,#2875,#2876));
#850=EDGE_LOOP('',(#2877,#2878,#2879,#2880,#2881,#2882));
#851=EDGE_LOOP('',(#2883));
#852=EDGE_LOOP('',(#2884));
#853=EDGE_LOOP('',(#2885,#2886,#2887,#2888));
#854=EDGE_LOOP('',(#2889,#2890,#2891,#2892));
#855=EDGE_LOOP('',(#2893,#2894,#2895,#2896));
#856=EDGE_LOOP('',(#2897,#2898,#2899,#2900));
#857=EDGE_LOOP('',(#2901,#2902,#2903,#2904));
#858=EDGE_LOOP('',(#2905,#2906,#2907,#2908));
#859=EDGE_LOOP('',(#2909));
#860=EDGE_LOOP('',(#2910,#2911,#2912,#2913));
#861=EDGE_LOOP('',(#2914));
#862=EDGE_LOOP('',(#2915,#2916,#2917,#2918));
#863=EDGE_LOOP('',(#2919,#2920,#2921,#2922,#2923,#2924));
#864=EDGE_LOOP('',(#2925));
#865=EDGE_LOOP('',(#2926));
#866=EDGE_LOOP('',(#2927,#2928,#2929,#2930));
#867=EDGE_LOOP('',(#2931,#2932,#2933,#2934));
#868=EDGE_LOOP('',(#2935,#2936,#2937,#2938));
#869=EDGE_LOOP('',(#2939,#2940,#2941,#2942,#2943,#2944));
#870=EDGE_LOOP('',(#2945,#2946,#2947,#2948,#2949,#2950));
#871=EDGE_LOOP('',(#2951));
#872=EDGE_LOOP('',(#2952));
#873=EDGE_LOOP('',(#2953));
#874=EDGE_LOOP('',(#2954));
#875=EDGE_LOOP('',(#2955));
#876=EDGE_LOOP('',(#2956));
#877=EDGE_LOOP('',(#2957));
#878=EDGE_LOOP('',(#2958));
#879=EDGE_LOOP('',(#2959));
#880=EDGE_LOOP('',(#2960));
#881=EDGE_LOOP('',(#2961));
#882=EDGE_LOOP('',(#2962));
#883=EDGE_LOOP('',(#2963,#2964,#2965,#2966));
#884=EDGE_LOOP('',(#2967,#2968,#2969,#2970));
#885=EDGE_LOOP('',(#2971));
#886=EDGE_LOOP('',(#2972));
#887=EDGE_LOOP('',(#2973));
#888=EDGE_LOOP('',(#2974));
#889=EDGE_LOOP('',(#2975,#2976,#2977,#2978));
#890=EDGE_LOOP('',(#2979,#2980,#2981,#2982));
#891=EDGE_LOOP('',(#2983,#2984,#2985,#2986));
#892=EDGE_LOOP('',(#2987,#2988,#2989,#2990));
#893=EDGE_LOOP('',(#2991,#2992,#2993,#2994));
#894=EDGE_LOOP('',(#2995));
#895=EDGE_LOOP('',(#2996));
#896=EDGE_LOOP('',(#2997,#2998,#2999,#3000));
#897=EDGE_LOOP('',(#3001));
#898=EDGE_LOOP('',(#3002));
#899=EDGE_LOOP('',(#3003,#3004,#3005,#3006));
#900=EDGE_LOOP('',(#3007,#3008,#3009,#3010));
#901=EDGE_LOOP('',(#3011));
#902=EDGE_LOOP('',(#3012));
#903=EDGE_LOOP('',(#3013));
#904=EDGE_LOOP('',(#3014));
#905=EDGE_LOOP('',(#3015));
#906=EDGE_LOOP('',(#3016));
#907=EDGE_LOOP('',(#3017));
#908=EDGE_LOOP('',(#3018));
#909=EDGE_LOOP('',(#3019));
#910=EDGE_LOOP('',(#3020));
#911=EDGE_LOOP('',(#3021));
#912=EDGE_LOOP('',(#3022));
#913=EDGE_LOOP('',(#3023,#3024,#3025,#3026));
#914=EDGE_LOOP('',(#3027,#3028,#3029,#3030));
#915=EDGE_LOOP('',(#3031));
#916=EDGE_LOOP('',(#3032));
#917=EDGE_LOOP('',(#3033));
#918=EDGE_LOOP('',(#3034));
#919=EDGE_LOOP('',(#3035,#3036,#3037,#3038));
#920=EDGE_LOOP('',(#3039));
#921=EDGE_LOOP('',(#3040));
#922=EDGE_LOOP('',(#3041,#3042,#3043,#3044));
#923=EDGE_LOOP('',(#3045));
#924=EDGE_LOOP('',(#3046));
#925=EDGE_LOOP('',(#3047,#3048,#3049,#3050));
#926=EDGE_LOOP('',(#3051));
#927=EDGE_LOOP('',(#3052));
#928=EDGE_LOOP('',(#3053,#3054,#3055,#3056));
#929=EDGE_LOOP('',(#3057));
#930=EDGE_LOOP('',(#3058));
#931=EDGE_LOOP('',(#3059,#3060,#3061,#3062));
#932=EDGE_LOOP('',(#3063,#3064,#3065,#3066));
#933=EDGE_LOOP('',(#3067,#3068,#3069,#3070));
#934=EDGE_LOOP('',(#3071,#3072,#3073,#3074));
#935=EDGE_LOOP('',(#3075));
#936=EDGE_LOOP('',(#3076));
#937=EDGE_LOOP('',(#3077,#3078,#3079,#3080));
#938=EDGE_LOOP('',(#3081,#3082,#3083,#3084));
#939=EDGE_LOOP('',(#3085));
#940=EDGE_LOOP('',(#3086));
#941=EDGE_LOOP('',(#3087,#3088,#3089,#3090));
#942=EDGE_LOOP('',(#3091));
#943=EDGE_LOOP('',(#3092,#3093,#3094,#3095));
#944=EDGE_LOOP('',(#3096));
#945=EDGE_LOOP('',(#3097));
#946=EDGE_LOOP('',(#3098));
#947=EDGE_LOOP('',(#3099));
#948=EDGE_LOOP('',(#3100));
#949=EDGE_LOOP('',(#3101));
#950=EDGE_LOOP('',(#3102));
#951=EDGE_LOOP('',(#3103));
#952=EDGE_LOOP('',(#3104));
#953=EDGE_LOOP('',(#3105));
#954=EDGE_LOOP('',(#3106));
#955=EDGE_LOOP('',(#3107,#3108,#3109,#3110));
#956=EDGE_LOOP('',(#3111,#3112,#3113,#3114));
#957=EDGE_LOOP('',(#3115,#3116,#3117,#3118));
#958=EDGE_LOOP('',(#3119,#3120,#3121,#3122));
#959=EDGE_LOOP('',(#3123,#3124,#3125,#3126));
#960=EDGE_LOOP('',(#3127,#3128,#3129,#3130));
#961=EDGE_LOOP('',(#3131,#3132,#3133,#3134));
#962=EDGE_LOOP('',(#3135,#3136,#3137,#3138));
#963=EDGE_LOOP('',(#3139,#3140,#3141,#3142));
#964=EDGE_LOOP('',(#3143,#3144,#3145,#3146));
#965=EDGE_LOOP('',(#3147,#3148,#3149,#3150));
#966=EDGE_LOOP('',(#3151,#3152,#3153,#3154));
#967=EDGE_LOOP('',(#3155,#3156,#3157,#3158,#3159,#3160));
#968=EDGE_LOOP('',(#3161,#3162,#3163,#3164,#3165));
#969=EDGE_LOOP('',(#3166,#3167,#3168,#3169));
#970=EDGE_LOOP('',(#3170,#3171,#3172,#3173));
#971=EDGE_LOOP('',(#3174));
#972=EDGE_LOOP('',(#3175));
#973=EDGE_LOOP('',(#3176,#3177,#3178,#3179,#3180));
#974=EDGE_LOOP('',(#3181));
#975=EDGE_LOOP('',(#3182));
#976=EDGE_LOOP('',(#3183,#3184,#3185,#3186));
#977=EDGE_LOOP('',(#3187,#3188,#3189,#3190,#3191,#3192));
#978=EDGE_LOOP('',(#3193,#3194,#3195,#3196,#3197));
#979=EDGE_LOOP('',(#3198));
#980=EDGE_LOOP('',(#3199));
#981=EDGE_LOOP('',(#3200,#3201,#3202,#3203));
#982=EDGE_LOOP('',(#3204,#3205,#3206,#3207));
#983=EDGE_LOOP('',(#3208,#3209,#3210,#3211));
#984=EDGE_LOOP('',(#3212));
#985=EDGE_LOOP('',(#3213));
#986=EDGE_LOOP('',(#3214,#3215,#3216,#3217,#3218));
#987=EDGE_LOOP('',(#3219,#3220));
#988=EDGE_LOOP('',(#3221,#3222));
#989=EDGE_LOOP('',(#3223,#3224));
#990=EDGE_LOOP('',(#3225,#3226));
#991=EDGE_LOOP('',(#3227,#3228));
#992=EDGE_LOOP('',(#3229,#3230));
#993=EDGE_LOOP('',(#3231,#3232));
#994=EDGE_LOOP('',(#3233,#3234));
#995=EDGE_LOOP('',(#3235,#3236,#3237,#3238));
#996=EDGE_LOOP('',(#3239,#3240,#3241,#3242,#3243,#3244,#3245,#3246,#3247,
#3248,#3249,#3250,#3251,#3252,#3253,#3254,#3255,#3256,#3257,#3258));
#997=EDGE_LOOP('',(#3259,#3260,#3261,#3262));
#998=EDGE_LOOP('',(#3263,#3264,#3265,#3266));
#999=EDGE_LOOP('',(#3267,#3268,#3269,#3270));
#1000=EDGE_LOOP('',(#3271,#3272,#3273,#3274));
#1001=EDGE_LOOP('',(#3275,#3276,#3277,#3278));
#1002=EDGE_LOOP('',(#3279,#3280,#3281,#3282,#3283,#3284));
#1003=EDGE_LOOP('',(#3285,#3286,#3287,#3288));
#1004=EDGE_LOOP('',(#3289,#3290,#3291,#3292));
#1005=EDGE_LOOP('',(#3293,#3294,#3295,#3296));
#1006=EDGE_LOOP('',(#3297,#3298,#3299,#3300));
#1007=EDGE_LOOP('',(#3301,#3302,#3303,#3304));
#1008=EDGE_LOOP('',(#3305,#3306,#3307,#3308));
#1009=EDGE_LOOP('',(#3309,#3310,#3311,#3312,#3313,#3314,#3315,#3316,#3317,
#3318,#3319,#3320,#3321,#3322,#3323,#3324,#3325,#3326,#3327,#3328));
#1010=EDGE_LOOP('',(#3329,#3330,#3331,#3332));
#1011=EDGE_LOOP('',(#3333,#3334,#3335,#3336));
#1012=EDGE_LOOP('',(#3337));
#1013=EDGE_LOOP('',(#3338));
#1014=EDGE_LOOP('',(#3339,#3340,#3341,#3342));
#1015=EDGE_LOOP('',(#3343));
#1016=EDGE_LOOP('',(#3344));
#1017=EDGE_LOOP('',(#3345,#3346,#3347,#3348));
#1018=EDGE_LOOP('',(#3349));
#1019=EDGE_LOOP('',(#3350));
#1020=EDGE_LOOP('',(#3351,#3352,#3353,#3354));
#1021=EDGE_LOOP('',(#3355));
#1022=EDGE_LOOP('',(#3356));
#1023=EDGE_LOOP('',(#3357,#3358,#3359,#3360));
#1024=EDGE_LOOP('',(#3361));
#1025=EDGE_LOOP('',(#3362));
#1026=EDGE_LOOP('',(#3363,#3364,#3365,#3366));
#1027=EDGE_LOOP('',(#3367));
#1028=EDGE_LOOP('',(#3368,#3369,#3370,#3371));
#1029=EDGE_LOOP('',(#3372,#3373,#3374,#3375));
#1030=EDGE_LOOP('',(#3376,#3377,#3378,#3379));
#1031=EDGE_LOOP('',(#3380));
#1032=EDGE_LOOP('',(#3381));
#1033=EDGE_LOOP('',(#3382,#3383,#3384,#3385));
#1034=EDGE_LOOP('',(#3386,#3387,#3388,#3389));
#1035=EDGE_LOOP('',(#3390,#3391,#3392,#3393));
#1036=EDGE_LOOP('',(#3394));
#1037=EDGE_LOOP('',(#3395,#3396,#3397,#3398));
#1038=EDGE_LOOP('',(#3399,#3400,#3401,#3402));
#1039=EDGE_LOOP('',(#3403,#3404,#3405,#3406));
#1040=EDGE_LOOP('',(#3407,#3408,#3409,#3410));
#1041=EDGE_LOOP('',(#3411,#3412,#3413,#3414));
#1042=EDGE_LOOP('',(#3415,#3416,#3417,#3418));
#1043=EDGE_LOOP('',(#3419,#3420,#3421,#3422,#3423,#3424));
#1044=EDGE_LOOP('',(#3425,#3426,#3427,#3428,#3429,#3430));
#1045=EDGE_LOOP('',(#3431));
#1046=EDGE_LOOP('',(#3432,#3433,#3434,#3435));
#1047=EDGE_LOOP('',(#3436,#3437,#3438,#3439));
#1048=EDGE_LOOP('',(#3440,#3441,#3442,#3443));
#1049=EDGE_LOOP('',(#3444));
#1050=EDGE_LOOP('',(#3445));
#1051=EDGE_LOOP('',(#3446,#3447,#3448,#3449));
#1052=EDGE_LOOP('',(#3450,#3451,#3452,#3453));
#1053=EDGE_LOOP('',(#3454,#3455,#3456,#3457));
#1054=EDGE_LOOP('',(#3458));
#1055=EDGE_LOOP('',(#3459,#3460,#3461,#3462));
#1056=EDGE_LOOP('',(#3463,#3464,#3465,#3466));
#1057=EDGE_LOOP('',(#3467,#3468,#3469,#3470));
#1058=EDGE_LOOP('',(#3471,#3472,#3473,#3474));
#1059=EDGE_LOOP('',(#3475,#3476,#3477,#3478));
#1060=EDGE_LOOP('',(#3479,#3480,#3481,#3482));
#1061=EDGE_LOOP('',(#3483,#3484,#3485,#3486,#3487,#3488));
#1062=EDGE_LOOP('',(#3489,#3490,#3491,#3492,#3493,#3494));
#1063=EDGE_LOOP('',(#3495,#3496,#3497,#3498));
#1064=EDGE_LOOP('',(#3499,#3500,#3501,#3502));
#1065=EDGE_LOOP('',(#3503,#3504,#3505,#3506));
#1066=EDGE_LOOP('',(#3507,#3508,#3509,#3510));
#1067=EDGE_LOOP('',(#3511,#3512,#3513,#3514));
#1068=EDGE_LOOP('',(#3515));
#1069=EDGE_LOOP('',(#3516));
#1070=EDGE_LOOP('',(#3517));
#1071=EDGE_LOOP('',(#3518));
#1072=EDGE_LOOP('',(#3519,#3520,#3521,#3522));
#1073=EDGE_LOOP('',(#3523,#3524,#3525,#3526));
#1074=EDGE_LOOP('',(#3527,#3528,#3529,#3530));
#1075=EDGE_LOOP('',(#3531,#3532,#3533,#3534));
#1076=EDGE_LOOP('',(#3535));
#1077=EDGE_LOOP('',(#3536));
#1078=EDGE_LOOP('',(#3537,#3538,#3539,#3540));
#1079=EDGE_LOOP('',(#3541,#3542,#3543,#3544));
#1080=EDGE_LOOP('',(#3545));
#1081=EDGE_LOOP('',(#3546));
#1082=EDGE_LOOP('',(#3547));
#1083=EDGE_LOOP('',(#3548));
#1084=EDGE_LOOP('',(#3549,#3550));
#1085=EDGE_LOOP('',(#3551,#3552,#3553,#3554,#3555,#3556,#3557,#3558,#3559));
#1086=EDGE_LOOP('',(#3560,#3561,#3562));
#1087=EDGE_LOOP('',(#3563,#3564,#3565,#3566));
#1088=EDGE_LOOP('',(#3567,#3568,#3569,#3570));
#1089=EDGE_LOOP('',(#3571,#3572,#3573,#3574));
#1090=EDGE_LOOP('',(#3575,#3576));
#1091=EDGE_LOOP('',(#3577));
#1092=EDGE_LOOP('',(#3578));
#1093=EDGE_LOOP('',(#3579));
#1094=EDGE_LOOP('',(#3580));
#1095=EDGE_LOOP('',(#3581,#3582));
#1096=EDGE_LOOP('',(#3583,#3584,#3585,#3586,#3587,#3588,#3589,#3590,#3591));
#1097=EDGE_LOOP('',(#3592,#3593,#3594));
#1098=EDGE_LOOP('',(#3595,#3596,#3597,#3598));
#1099=EDGE_LOOP('',(#3599,#3600,#3601,#3602));
#1100=EDGE_LOOP('',(#3603,#3604,#3605,#3606));
#1101=EDGE_LOOP('',(#3607));
#1102=EDGE_LOOP('',(#3608,#3609,#3610,#3611));
#1103=EDGE_LOOP('',(#3612,#3613,#3614,#3615));
#1104=EDGE_LOOP('',(#3616,#3617,#3618,#3619));
#1105=EDGE_LOOP('',(#3620,#3621,#3622,#3623));
#1106=EDGE_LOOP('',(#3624,#3625,#3626,#3627));
#1107=EDGE_LOOP('',(#3628,#3629,#3630,#3631));
#1108=EDGE_LOOP('',(#3632,#3633,#3634,#3635));
#1109=EDGE_LOOP('',(#3636));
#1110=EDGE_LOOP('',(#3637));
#1111=EDGE_LOOP('',(#3638));
#1112=EDGE_LOOP('',(#3639));
#1113=EDGE_LOOP('',(#3640));
#1114=EDGE_LOOP('',(#3641));
#1115=EDGE_LOOP('',(#3642,#3643,#3644,#3645));
#1116=EDGE_LOOP('',(#3646,#3647,#3648,#3649));
#1117=EDGE_LOOP('',(#3650,#3651));
#1118=EDGE_LOOP('',(#3652));
#1119=EDGE_LOOP('',(#3653,#3654,#3655,#3656));
#1120=EDGE_LOOP('',(#3657));
#1121=EDGE_LOOP('',(#3658));
#1122=EDGE_LOOP('',(#3659));
#1123=EDGE_LOOP('',(#3660));
#1124=EDGE_LOOP('',(#3661,#3662,#3663,#3664,#3665,#3666,#3667,#3668));
#1125=EDGE_LOOP('',(#3669,#3670,#3671,#3672));
#1126=EDGE_LOOP('',(#3673,#3674,#3675,#3676));
#1127=EDGE_LOOP('',(#3677,#3678,#3679,#3680));
#1128=EDGE_LOOP('',(#3681,#3682,#3683,#3684));
#1129=EDGE_LOOP('',(#3685,#3686,#3687,#3688,#3689,#3690,#3691,#3692));
#1130=EDGE_LOOP('',(#3693,#3694,#3695,#3696));
#1131=EDGE_LOOP('',(#3697,#3698,#3699,#3700));
#1132=EDGE_LOOP('',(#3701,#3702,#3703,#3704));
#1133=EDGE_LOOP('',(#3705,#3706,#3707,#3708));
#1134=EDGE_LOOP('',(#3709,#3710,#3711,#3712));
#1135=EDGE_LOOP('',(#3713,#3714,#3715,#3716));
#1136=EDGE_LOOP('',(#3717,#3718,#3719,#3720));
#1137=EDGE_LOOP('',(#3721,#3722,#3723,#3724));
#1138=EDGE_LOOP('',(#3725,#3726,#3727,#3728));
#1139=EDGE_LOOP('',(#3729,#3730,#3731,#3732));
#1140=EDGE_LOOP('',(#3733,#3734,#3735,#3736,#3737,#3738));
#1141=EDGE_LOOP('',(#3739));
#1142=EDGE_LOOP('',(#3740,#3741,#3742,#3743,#3744,#3745));
#1143=EDGE_LOOP('',(#3746,#3747,#3748,#3749));
#1144=EDGE_LOOP('',(#3750,#3751,#3752,#3753));
#1145=EDGE_LOOP('',(#3754,#3755,#3756,#3757));
#1146=EDGE_LOOP('',(#3758));
#1147=LINE('',#6213,#1409);
#1148=LINE('',#6219,#1410);
#1149=LINE('',#6225,#1411);
#1150=LINE('',#6231,#1412);
#1151=LINE('',#6236,#1413);
#1152=LINE('',#6238,#1414);
#1153=LINE('',#6240,#1415);
#1154=LINE('',#6241,#1416);
#1155=LINE('',#6244,#1417);
#1156=LINE('',#6246,#1418);
#1157=LINE('',#6247,#1419);
#1158=LINE('',#6250,#1420);
#1159=LINE('',#6252,#1421);
#1160=LINE('',#6253,#1422);
#1161=LINE('',#6255,#1423);
#1162=LINE('',#6256,#1424);
#1163=LINE('',#6264,#1425);
#1164=LINE('',#6271,#1426);
#1165=LINE('',#6278,#1427);
#1166=LINE('',#6285,#1428);
#1167=LINE('',#6292,#1429);
#1168=LINE('',#6299,#1430);
#1169=LINE('',#6306,#1431);
#1170=LINE('',#6313,#1432);
#1171=LINE('',#6320,#1433);
#1172=LINE('',#6326,#1434);
#1173=LINE('',#6332,#1435);
#1174=LINE('',#6338,#1436);
#1175=LINE('',#6345,#1437);
#1176=LINE('',#6347,#1438);
#1177=LINE('',#6348,#1439);
#1178=LINE('',#6353,#1440);
#1179=LINE('',#6355,#1441);
#1180=LINE('',#6356,#1442);
#1181=LINE('',#6362,#1443);
#1182=LINE('',#6364,#1444);
#1183=LINE('',#6365,#1445);
#1184=LINE('',#6370,#1446);
#1185=LINE('',#6372,#1447);
#1186=LINE('',#6373,#1448);
#1187=LINE('',#6375,#1449);
#1188=LINE('',#6376,#1450);
#1189=LINE('',#6378,#1451);
#1190=LINE('',#6379,#1452);
#1191=LINE('',#6381,#1453);
#1192=LINE('',#6383,#1454);
#1193=LINE('',#6390,#1455);
#1194=LINE('',#6392,#1456);
#1195=LINE('',#6393,#1457);
#1196=LINE('',#6398,#1458);
#1197=LINE('',#6400,#1459);
#1198=LINE('',#6401,#1460);
#1199=LINE('',#6407,#1461);
#1200=LINE('',#6409,#1462);
#1201=LINE('',#6410,#1463);
#1202=LINE('',#6415,#1464);
#1203=LINE('',#6417,#1465);
#1204=LINE('',#6418,#1466);
#1205=LINE('',#6420,#1467);
#1206=LINE('',#6421,#1468);
#1207=LINE('',#6423,#1469);
#1208=LINE('',#6424,#1470);
#1209=LINE('',#6426,#1471);
#1210=LINE('',#6428,#1472);
#1211=LINE('',#6434,#1473);
#1212=LINE('',#6440,#1474);
#1213=LINE('',#6449,#1475);
#1214=LINE('',#6455,#1476);
#1215=LINE('',#6464,#1477);
#1216=LINE('',#6470,#1478);
#1217=LINE('',#6476,#1479);
#1218=LINE('',#6482,#1480);
#1219=LINE('',#6488,#1481);
#1220=LINE('',#6497,#1482);
#1221=LINE('',#6503,#1483);
#1222=LINE('',#6508,#1484);
#1223=LINE('',#6517,#1485);
#1224=LINE('',#6523,#1486);
#1225=LINE('',#6532,#1487);
#1226=LINE('',#6541,#1488);
#1227=LINE('',#6550,#1489);
#1228=LINE('',#6559,#1490);
#1229=LINE('',#6567,#1491);
#1230=LINE('',#6571,#1492);
#1231=LINE('',#6575,#1493);
#1232=LINE('',#6579,#1494);
#1233=LINE('',#6587,#1495);
#1234=LINE('',#6593,#1496);
#1235=LINE('',#6598,#1497);
#1236=LINE('',#6605,#1498);
#1237=LINE('',#6613,#1499);
#1238=LINE('',#6615,#1500);
#1239=LINE('',#6617,#1501);
#1240=LINE('',#6618,#1502);
#1241=LINE('',#6621,#1503);
#1242=LINE('',#6623,#1504);
#1243=LINE('',#6624,#1505);
#1244=LINE('',#6627,#1506);
#1245=LINE('',#6629,#1507);
#1246=LINE('',#6630,#1508);
#1247=LINE('',#6632,#1509);
#1248=LINE('',#6633,#1510);
#1249=LINE('',#6640,#1511);
#1250=LINE('',#6642,#1512);
#1251=LINE('',#6644,#1513);
#1252=LINE('',#6645,#1514);
#1253=LINE('',#6648,#1515);
#1254=LINE('',#6650,#1516);
#1255=LINE('',#6651,#1517);
#1256=LINE('',#6654,#1518);
#1257=LINE('',#6656,#1519);
#1258=LINE('',#6657,#1520);
#1259=LINE('',#6659,#1521);
#1260=LINE('',#6660,#1522);
#1261=LINE('',#6677,#1523);
#1262=LINE('',#6683,#1524);
#1263=LINE('',#6687,#1525);
#1264=LINE('',#6693,#1526);
#1265=LINE('',#6698,#1527);
#1266=LINE('',#6713,#1528);
#1267=LINE('',#6722,#1529);
#1268=LINE('',#6726,#1530);
#1269=LINE('',#6730,#1531);
#1270=LINE('',#6733,#1532);
#1271=LINE('',#6886,#1533);
#1272=LINE('',#7182,#1534);
#1273=LINE('',#7224,#1535);
#1274=LINE('',#7229,#1536);
#1275=LINE('',#7238,#1537);
#1276=LINE('',#7243,#1538);
#1277=LINE('',#7256,#1539);
#1278=LINE('',#7260,#1540);
#1279=LINE('',#7264,#1541);
#1280=LINE('',#7271,#1542);
#1281=LINE('',#7275,#1543);
#1282=LINE('',#7279,#1544);
#1283=LINE('',#7284,#1545);
#1284=LINE('',#7286,#1546);
#1285=LINE('',#7288,#1547);
#1286=LINE('',#7289,#1548);
#1287=LINE('',#7292,#1549);
#1288=LINE('',#7294,#1550);
#1289=LINE('',#7295,#1551);
#1290=LINE('',#7298,#1552);
#1291=LINE('',#7300,#1553);
#1292=LINE('',#7301,#1554);
#1293=LINE('',#7304,#1555);
#1294=LINE('',#7306,#1556);
#1295=LINE('',#7307,#1557);
#1296=LINE('',#7310,#1558);
#1297=LINE('',#7312,#1559);
#1298=LINE('',#7313,#1560);
#1299=LINE('',#7315,#1561);
#1300=LINE('',#7316,#1562);
#1301=LINE('',#7326,#1563);
#1302=LINE('',#7330,#1564);
#1303=LINE('',#7334,#1565);
#1304=LINE('',#7341,#1566);
#1305=LINE('',#7345,#1567);
#1306=LINE('',#7349,#1568);
#1307=LINE('',#7354,#1569);
#1308=LINE('',#7356,#1570);
#1309=LINE('',#7358,#1571);
#1310=LINE('',#7359,#1572);
#1311=LINE('',#7362,#1573);
#1312=LINE('',#7364,#1574);
#1313=LINE('',#7365,#1575);
#1314=LINE('',#7368,#1576);
#1315=LINE('',#7370,#1577);
#1316=LINE('',#7371,#1578);
#1317=LINE('',#7374,#1579);
#1318=LINE('',#7376,#1580);
#1319=LINE('',#7377,#1581);
#1320=LINE('',#7380,#1582);
#1321=LINE('',#7382,#1583);
#1322=LINE('',#7383,#1584);
#1323=LINE('',#7385,#1585);
#1324=LINE('',#7386,#1586);
#1325=LINE('',#7416,#1587);
#1326=LINE('',#7418,#1588);
#1327=LINE('',#7420,#1589);
#1328=LINE('',#7421,#1590);
#1329=LINE('',#7426,#1591);
#1330=LINE('',#7427,#1592);
#1331=LINE('',#7430,#1593);
#1332=LINE('',#7432,#1594);
#1333=LINE('',#7433,#1595);
#1334=LINE('',#7435,#1596);
#1335=LINE('',#7449,#1597);
#1336=LINE('',#7452,#1598);
#1337=LINE('',#7457,#1599);
#1338=LINE('',#7465,#1600);
#1339=LINE('',#7471,#1601);
#1340=LINE('',#7479,#1602);
#1341=LINE('',#7500,#1603);
#1342=LINE('',#7555,#1604);
#1343=LINE('',#7560,#1605);
#1344=LINE('',#7566,#1606);
#1345=LINE('',#7574,#1607);
#1346=LINE('',#7591,#1608);
#1347=LINE('',#7642,#1609);
#1348=LINE('',#7646,#1610);
#1349=LINE('',#7648,#1611);
#1350=LINE('',#7650,#1612);
#1351=LINE('',#7651,#1613);
#1352=LINE('',#7654,#1614);
#1353=LINE('',#7656,#1615);
#1354=LINE('',#7657,#1616);
#1355=LINE('',#7660,#1617);
#1356=LINE('',#7662,#1618);
#1357=LINE('',#7663,#1619);
#1358=LINE('',#7674,#1620);
#1359=LINE('',#7680,#1621);
#1360=LINE('',#7686,#1622);
#1361=LINE('',#7692,#1623);
#1362=LINE('',#7701,#1624);
#1363=LINE('',#7704,#1625);
#1364=LINE('',#7710,#1626);
#1365=LINE('',#7712,#1627);
#1366=LINE('',#7714,#1628);
#1367=LINE('',#7716,#1629);
#1368=LINE('',#7718,#1630);
#1369=LINE('',#7720,#1631);
#1370=LINE('',#7722,#1632);
#1371=LINE('',#7723,#1633);
#1372=LINE('',#7726,#1634);
#1373=LINE('',#7728,#1635);
#1374=LINE('',#7729,#1636);
#1375=LINE('',#7732,#1637);
#1376=LINE('',#7733,#1638);
#1377=LINE('',#7736,#1639);
#1378=LINE('',#7737,#1640);
#1379=LINE('',#7740,#1641);
#1380=LINE('',#7741,#1642);
#1381=LINE('',#7745,#1643);
#1382=LINE('',#7746,#1644);
#1383=LINE('',#7748,#1645);
#1384=LINE('',#7749,#1646);
#1385=LINE('',#7751,#1647);
#1386=LINE('',#7753,#1648);
#1387=LINE('',#7755,#1649);
#1388=LINE('',#7761,#1650);
#1389=LINE('',#7763,#1651);
#1390=LINE('',#7765,#1652);
#1391=LINE('',#7766,#1653);
#1392=LINE('',#7769,#1654);
#1393=LINE('',#7771,#1655);
#1394=LINE('',#7772,#1656);
#1395=LINE('',#7775,#1657);
#1396=LINE('',#7777,#1658);
#1397=LINE('',#7778,#1659);
#1398=LINE('',#7781,#1660);
#1399=LINE('',#7783,#1661);
#1400=LINE('',#7784,#1662);
#1401=LINE('',#7787,#1663);
#1402=LINE('',#7789,#1664);
#1403=LINE('',#7790,#1665);
#1404=LINE('',#7792,#1666);
#1405=LINE('',#7793,#1667);
#1406=LINE('',#7801,#1668);
#1407=LINE('',#7805,#1669);
#1408=LINE('',#7809,#1670);
#1409=VECTOR('',#4890,0.25);
#1410=VECTOR('',#4897,0.25);
#1411=VECTOR('',#4904,0.25);
#1412=VECTOR('',#4911,0.25);
#1413=VECTOR('',#4916,1.);
#1414=VECTOR('',#4917,1.);
#1415=VECTOR('',#4918,1.);
#1416=VECTOR('',#4919,1.);
#1417=VECTOR('',#4922,1.);
#1418=VECTOR('',#4923,1.);
#1419=VECTOR('',#4924,1.);
#1420=VECTOR('',#4927,1.);
#1421=VECTOR('',#4928,1.);
#1422=VECTOR('',#4929,1.);
#1423=VECTOR('',#4932,1.);
#1424=VECTOR('',#4933,1.);
#1425=VECTOR('',#4944,0.165);
#1426=VECTOR('',#4953,0.165);
#1427=VECTOR('',#4962,0.165);
#1428=VECTOR('',#4971,0.165);
#1429=VECTOR('',#4980,0.165);
#1430=VECTOR('',#4989,0.165);
#1431=VECTOR('',#4998,0.165);
#1432=VECTOR('',#5007,0.165);
#1433=VECTOR('',#5016,0.33);
#1434=VECTOR('',#5023,0.33);
#1435=VECTOR('',#5030,0.33);
#1436=VECTOR('',#5037,0.33);
#1437=VECTOR('',#5044,1.);
#1438=VECTOR('',#5045,1.);
#1439=VECTOR('',#5046,1.);
#1440=VECTOR('',#5051,1.);
#1441=VECTOR('',#5052,1.);
#1442=VECTOR('',#5053,1.);
#1443=VECTOR('',#5058,1.);
#1444=VECTOR('',#5059,1.);
#1445=VECTOR('',#5060,1.);
#1446=VECTOR('',#5065,1.);
#1447=VECTOR('',#5066,1.);
#1448=VECTOR('',#5067,1.);
#1449=VECTOR('',#5070,1.);
#1450=VECTOR('',#5071,1.);
#1451=VECTOR('',#5074,1.);
#1452=VECTOR('',#5075,1.);
#1453=VECTOR('',#5078,1.);
#1454=VECTOR('',#5081,1.);
#1455=VECTOR('',#5088,1.);
#1456=VECTOR('',#5089,1.);
#1457=VECTOR('',#5090,1.);
#1458=VECTOR('',#5095,1.);
#1459=VECTOR('',#5096,1.);
#1460=VECTOR('',#5097,1.);
#1461=VECTOR('',#5102,1.);
#1462=VECTOR('',#5103,1.);
#1463=VECTOR('',#5104,1.);
#1464=VECTOR('',#5109,1.);
#1465=VECTOR('',#5110,1.);
#1466=VECTOR('',#5111,1.);
#1467=VECTOR('',#5114,1.);
#1468=VECTOR('',#5115,1.);
#1469=VECTOR('',#5118,1.);
#1470=VECTOR('',#5119,1.);
#1471=VECTOR('',#5122,1.);
#1472=VECTOR('',#5125,1.);
#1473=VECTOR('',#5132,2.35);
#1474=VECTOR('',#5139,3.5);
#1475=VECTOR('',#5152,1.75);
#1476=VECTOR('',#5159,2.34);
#1477=VECTOR('',#5172,0.225);
#1478=VECTOR('',#5179,0.225);
#1479=VECTOR('',#5186,0.225);
#1480=VECTOR('',#5193,0.225);
#1481=VECTOR('',#5200,2.34);
#1482=VECTOR('',#5211,1.8);
#1483=VECTOR('',#5220,1.6);
#1484=VECTOR('',#5225,3.5);
#1485=VECTOR('',#5238,1.);
#1486=VECTOR('',#5245,1.8);
#1487=VECTOR('',#5258,0.4);
#1488=VECTOR('',#5269,0.4);
#1489=VECTOR('',#5280,0.4);
#1490=VECTOR('',#5291,0.4);
#1491=VECTOR('',#5302,0.225);
#1492=VECTOR('',#5307,0.225);
#1493=VECTOR('',#5312,0.225);
#1494=VECTOR('',#5317,0.225);
#1495=VECTOR('',#5326,1.8);
#1496=VECTOR('',#5333,2.34);
#1497=VECTOR('',#5340,2.);
#1498=VECTOR('',#5349,3.5);
#1499=VECTOR('',#5360,1.);
#1500=VECTOR('',#5361,1.);
#1501=VECTOR('',#5362,1.);
#1502=VECTOR('',#5363,1.);
#1503=VECTOR('',#5366,1.);
#1504=VECTOR('',#5367,1.);
#1505=VECTOR('',#5368,1.);
#1506=VECTOR('',#5371,1.);
#1507=VECTOR('',#5372,1.);
#1508=VECTOR('',#5373,1.);
#1509=VECTOR('',#5376,1.);
#1510=VECTOR('',#5377,1.);
#1511=VECTOR('',#5386,1.);
#1512=VECTOR('',#5387,1.);
#1513=VECTOR('',#5388,1.);
#1514=VECTOR('',#5389,1.);
#1515=VECTOR('',#5392,1.);
#1516=VECTOR('',#5393,1.);
#1517=VECTOR('',#5394,1.);
#1518=VECTOR('',#5397,1.);
#1519=VECTOR('',#5398,1.);
#1520=VECTOR('',#5399,1.);
#1521=VECTOR('',#5402,1.);
#1522=VECTOR('',#5403,1.);
#1523=VECTOR('',#5426,1.63531);
#1524=VECTOR('',#5433,1.);
#1525=VECTOR('',#5438,1.05);
#1526=VECTOR('',#5447,1.63531);
#1527=VECTOR('',#5454,1.05);
#1528=VECTOR('',#5473,1.71469);
#1529=VECTOR('',#5484,2.3);
#1530=VECTOR('',#5489,2.35);
#1531=VECTOR('',#5494,2.3);
#1532=VECTOR('',#5499,1.71469);
#1533=VECTOR('',#5550,1.706752);
#1534=VECTOR('',#5627,1.643248);
#1535=VECTOR('',#5656,1.70469);
#1536=VECTOR('',#5663,1.65031);
#1537=VECTOR('',#5674,1.70469);
#1538=VECTOR('',#5681,1.65031);
#1539=VECTOR('',#5702,0.475);
#1540=VECTOR('',#5707,0.5);
#1541=VECTOR('',#5712,0.485);
#1542=VECTOR('',#5721,0.31);
#1543=VECTOR('',#5726,0.3);
#1544=VECTOR('',#5731,0.27);
#1545=VECTOR('',#5736,1.);
#1546=VECTOR('',#5737,1.);
#1547=VECTOR('',#5738,1.);
#1548=VECTOR('',#5739,1.);
#1549=VECTOR('',#5742,1.);
#1550=VECTOR('',#5743,1.);
#1551=VECTOR('',#5744,1.);
#1552=VECTOR('',#5747,1.);
#1553=VECTOR('',#5748,1.);
#1554=VECTOR('',#5749,1.);
#1555=VECTOR('',#5752,1.);
#1556=VECTOR('',#5753,1.);
#1557=VECTOR('',#5754,1.);
#1558=VECTOR('',#5757,1.);
#1559=VECTOR('',#5758,1.);
#1560=VECTOR('',#5759,1.);
#1561=VECTOR('',#5762,1.);
#1562=VECTOR('',#5763,1.);
#1563=VECTOR('',#5778,0.325);
#1564=VECTOR('',#5783,0.35);
#1565=VECTOR('',#5788,0.335);
#1566=VECTOR('',#5797,0.21);
#1567=VECTOR('',#5802,0.2);
#1568=VECTOR('',#5807,0.18);
#1569=VECTOR('',#5812,1.);
#1570=VECTOR('',#5813,1.);
#1571=VECTOR('',#5814,1.);
#1572=VECTOR('',#5815,1.);
#1573=VECTOR('',#5818,1.);
#1574=VECTOR('',#5819,1.);
#1575=VECTOR('',#5820,1.);
#1576=VECTOR('',#5823,1.);
#1577=VECTOR('',#5824,1.);
#1578=VECTOR('',#5825,1.);
#1579=VECTOR('',#5828,1.);
#1580=VECTOR('',#5829,1.);
#1581=VECTOR('',#5830,1.);
#1582=VECTOR('',#5833,1.);
#1583=VECTOR('',#5834,1.);
#1584=VECTOR('',#5835,1.);
#1585=VECTOR('',#5838,1.);
#1586=VECTOR('',#5839,1.);
#1587=VECTOR('',#5894,1.);
#1588=VECTOR('',#5895,1.);
#1589=VECTOR('',#5896,1.);
#1590=VECTOR('',#5897,1.);
#1591=VECTOR('',#5902,1.);
#1592=VECTOR('',#5903,1.);
#1593=VECTOR('',#5906,1.);
#1594=VECTOR('',#5907,1.);
#1595=VECTOR('',#5908,1.);
#1596=VECTOR('',#5911,1.);
#1597=VECTOR('',#5930,1.2);
#1598=VECTOR('',#5933,1.);
#1599=VECTOR('',#5940,1.);
#1600=VECTOR('',#5951,1.01);
#1601=VECTOR('',#5958,1.35);
#1602=VECTOR('',#5969,1.);
#1603=VECTOR('',#5976,0.21);
#1604=VECTOR('',#5981,1.);
#1605=VECTOR('',#5986,1.005);
#1606=VECTOR('',#5993,1.5);
#1607=VECTOR('',#6004,1.);
#1608=VECTOR('',#6011,0.21);
#1609=VECTOR('',#6016,1.);
#1610=VECTOR('',#6019,1.);
#1611=VECTOR('',#6020,1.);
#1612=VECTOR('',#6021,1.);
#1613=VECTOR('',#6022,1.);
#1614=VECTOR('',#6025,1.);
#1615=VECTOR('',#6026,1.);
#1616=VECTOR('',#6027,1.);
#1617=VECTOR('',#6030,1.);
#1618=VECTOR('',#6031,1.);
#1619=VECTOR('',#6032,1.);
#1620=VECTOR('',#6047,0.33);
#1621=VECTOR('',#6054,0.33);
#1622=VECTOR('',#6061,0.33);
#1623=VECTOR('',#6068,0.33);
#1624=VECTOR('',#6079,3.5);
#1625=VECTOR('',#6084,1.6);
#1626=VECTOR('',#6091,1.);
#1627=VECTOR('',#6092,1.);
#1628=VECTOR('',#6093,1.);
#1629=VECTOR('',#6094,1.);
#1630=VECTOR('',#6095,1.);
#1631=VECTOR('',#6096,1.);
#1632=VECTOR('',#6097,1.);
#1633=VECTOR('',#6098,1.);
#1634=VECTOR('',#6101,1.);
#1635=VECTOR('',#6102,1.);
#1636=VECTOR('',#6103,1.);
#1637=VECTOR('',#6106,1.);
#1638=VECTOR('',#6107,1.);
#1639=VECTOR('',#6110,1.);
#1640=VECTOR('',#6111,1.);
#1641=VECTOR('',#6114,1.);
#1642=VECTOR('',#6115,1.);
#1643=VECTOR('',#6118,1.);
#1644=VECTOR('',#6119,1.);
#1645=VECTOR('',#6120,1.);
#1646=VECTOR('',#6121,1.);
#1647=VECTOR('',#6124,1.);
#1648=VECTOR('',#6127,1.);
#1649=VECTOR('',#6130,1.);
#1650=VECTOR('',#6137,1.);
#1651=VECTOR('',#6138,1.);
#1652=VECTOR('',#6139,1.);
#1653=VECTOR('',#6140,1.);
#1654=VECTOR('',#6143,1.);
#1655=VECTOR('',#6144,1.);
#1656=VECTOR('',#6145,1.);
#1657=VECTOR('',#6148,1.);
#1658=VECTOR('',#6149,1.);
#1659=VECTOR('',#6150,1.);
#1660=VECTOR('',#6153,1.);
#1661=VECTOR('',#6154,1.);
#1662=VECTOR('',#6155,1.);
#1663=VECTOR('',#6158,1.);
#1664=VECTOR('',#6159,1.);
#1665=VECTOR('',#6160,1.);
#1666=VECTOR('',#6163,1.);
#1667=VECTOR('',#6164,1.);
#1668=VECTOR('',#6175,0.235);
#1669=VECTOR('',#6180,0.25);
#1670=VECTOR('',#6185,0.2125);
#1671=CIRCLE('',#4352,0.25);
#1672=CIRCLE('',#4353,0.25);
#1673=CIRCLE('',#4355,0.25);
#1674=CIRCLE('',#4356,0.25);
#1675=CIRCLE('',#4358,0.25);
#1676=CIRCLE('',#4359,0.25);
#1677=CIRCLE('',#4361,0.25);
#1678=CIRCLE('',#4362,0.25);
#1679=CIRCLE('',#4371,0.165);
#1680=CIRCLE('',#4372,0.165);
#1681=CIRCLE('',#4375,0.165);
#1682=CIRCLE('',#4376,0.165);
#1683=CIRCLE('',#4379,0.165);
#1684=CIRCLE('',#4380,0.165);
#1685=CIRCLE('',#4383,0.165);
#1686=CIRCLE('',#4384,0.165);
#1687=CIRCLE('',#4387,0.165);
#1688=CIRCLE('',#4388,0.165);
#1689=CIRCLE('',#4391,0.165);
#1690=CIRCLE('',#4392,0.165);
#1691=CIRCLE('',#4395,0.165);
#1692=CIRCLE('',#4396,0.165);
#1693=CIRCLE('',#4399,0.165);
#1694=CIRCLE('',#4400,0.165);
#1695=CIRCLE('',#4403,0.33);
#1696=CIRCLE('',#4404,0.33);
#1697=CIRCLE('',#4406,0.33);
#1698=CIRCLE('',#4407,0.33);
#1699=CIRCLE('',#4409,0.33);
#1700=CIRCLE('',#4410,0.33);
#1701=CIRCLE('',#4412,0.33);
#1702=CIRCLE('',#4413,0.33);
#1703=CIRCLE('',#4415,3.5);
#1704=CIRCLE('',#4417,3.5);
#1705=CIRCLE('',#4419,3.5);
#1706=CIRCLE('',#4421,3.5);
#1707=CIRCLE('',#4428,3.5);
#1708=CIRCLE('',#4430,3.5);
#1709=CIRCLE('',#4432,3.5);
#1710=CIRCLE('',#4434,3.5);
#1711=CIRCLE('',#4441,2.35);
#1712=CIRCLE('',#4442,2.35);
#1713=CIRCLE('',#4444,3.5);
#1714=CIRCLE('',#4445,3.5);
#1715=CIRCLE('',#4450,1.75);
#1716=CIRCLE('',#4451,1.75);
#1717=CIRCLE('',#4453,2.34);
#1718=CIRCLE('',#4454,2.34);
#1719=CIRCLE('',#4459,0.225);
#1720=CIRCLE('',#4460,0.225);
#1721=CIRCLE('',#4462,0.225);
#1722=CIRCLE('',#4463,0.225);
#1723=CIRCLE('',#4465,0.225);
#1724=CIRCLE('',#4466,0.225);
#1725=CIRCLE('',#4468,0.225);
#1726=CIRCLE('',#4469,0.225);
#1727=CIRCLE('',#4471,2.34);
#1728=CIRCLE('',#4472,2.34);
#1729=CIRCLE('',#4474,1.6);
#1730=CIRCLE('',#4476,1.8);
#1731=CIRCLE('',#4477,1.8);
#1732=CIRCLE('',#4479,1.6);
#1733=CIRCLE('',#4482,3.5);
#1734=CIRCLE('',#4483,3.5);
#1735=CIRCLE('',#4488,1.);
#1736=CIRCLE('',#4489,1.);
#1737=CIRCLE('',#4491,1.8);
#1738=CIRCLE('',#4492,1.8);
#1739=CIRCLE('',#4497,0.4);
#1740=CIRCLE('',#4498,0.4);
#1741=CIRCLE('',#4500,0.225);
#1742=CIRCLE('',#4502,0.4);
#1743=CIRCLE('',#4503,0.4);
#1744=CIRCLE('',#4505,0.225);
#1745=CIRCLE('',#4507,0.4);
#1746=CIRCLE('',#4508,0.4);
#1747=CIRCLE('',#4510,0.225);
#1748=CIRCLE('',#4512,0.4);
#1749=CIRCLE('',#4513,0.4);
#1750=CIRCLE('',#4515,0.225);
#1751=CIRCLE('',#4517,0.225);
#1752=CIRCLE('',#4519,0.225);
#1753=CIRCLE('',#4521,0.225);
#1754=CIRCLE('',#4523,0.225);
#1755=CIRCLE('',#4525,2.);
#1756=CIRCLE('',#4526,1.8);
#1757=CIRCLE('',#4528,1.8);
#1758=CIRCLE('',#4530,2.34);
#1759=CIRCLE('',#4531,2.34);
#1760=CIRCLE('',#4534,2.);
#1761=CIRCLE('',#4537,3.5);
#1762=CIRCLE('',#4538,3.5);
#1763=CIRCLE('',#4558,1.63531);
#1764=CIRCLE('',#4559,1.63531);
#1765=CIRCLE('',#4560,0.412776);
#1766=CIRCLE('',#4561,1.63531);
#1767=CIRCLE('',#4562,1.63531);
#1768=CIRCLE('',#4564,1.63531);
#1769=CIRCLE('',#4566,1.);
#1770=CIRCLE('',#4567,1.);
#1771=CIRCLE('',#4569,1.1);
#1772=CIRCLE('',#4572,1.63531);
#1773=CIRCLE('',#4574,1.1);
#1774=CIRCLE('',#4578,1.71469);
#1775=CIRCLE('',#4579,1.71469);
#1776=CIRCLE('',#4580,0.412776);
#1777=CIRCLE('',#4581,1.71469);
#1778=CIRCLE('',#4582,1.71469);
#1779=CIRCLE('',#4584,1.71469);
#1780=CIRCLE('',#4586,2.25);
#1781=CIRCLE('',#4587,1.71469);
#1782=CIRCLE('',#4589,2.35);
#1783=CIRCLE('',#4591,2.35);
#1784=CIRCLE('',#4593,2.25);
#1785=CIRCLE('',#4598,0.3969);
#1786=CIRCLE('',#4600,0.3969);
#1787=CIRCLE('',#4602,0.3969);
#1788=CIRCLE('',#4604,0.3969);
#1789=CIRCLE('',#4606,0.3969);
#1790=CIRCLE('',#4608,0.3969);
#1791=CIRCLE('',#4610,0.3969);
#1792=CIRCLE('',#4612,0.3969);
#1793=CIRCLE('',#4615,0.405071403305639);
#1794=CIRCLE('',#4616,0.405071403305639);
#1795=CIRCLE('',#4618,1.706752);
#1796=CIRCLE('',#4619,1.706752);
#1797=CIRCLE('',#4620,1.706752);
#1798=CIRCLE('',#4621,1.706752);
#1799=CIRCLE('',#4622,1.706752);
#1800=CIRCLE('',#4623,1.706752);
#1801=CIRCLE('',#4624,1.706752);
#1802=CIRCLE('',#4625,1.706752);
#1803=CIRCLE('',#4626,1.706752);
#1804=CIRCLE('',#4628,1.643248);
#1805=CIRCLE('',#4629,0.405071403305639);
#1806=CIRCLE('',#4631,0.405071403305639);
#1807=CIRCLE('',#4633,1.643248);
#1808=CIRCLE('',#4634,0.405071403305639);
#1809=CIRCLE('',#4636,0.405071403305639);
#1810=CIRCLE('',#4638,1.643248);
#1811=CIRCLE('',#4639,0.405071403305639);
#1812=CIRCLE('',#4641,0.405071403305639);
#1813=CIRCLE('',#4643,1.643248);
#1814=CIRCLE('',#4644,0.405071403305639);
#1815=CIRCLE('',#4646,0.405071403305639);
#1816=CIRCLE('',#4648,1.643248);
#1817=CIRCLE('',#4649,0.405071403305639);
#1818=CIRCLE('',#4651,0.405071403305639);
#1819=CIRCLE('',#4653,1.643248);
#1820=CIRCLE('',#4654,0.405071403305639);
#1821=CIRCLE('',#4656,0.405071403305639);
#1822=CIRCLE('',#4658,1.643248);
#1823=CIRCLE('',#4659,1.643248);
#1824=CIRCLE('',#4660,1.643248);
#1825=CIRCLE('',#4662,0.405071403305639);
#1826=CIRCLE('',#4664,0.405071403305639);
#1827=CIRCLE('',#4669,1.70469);
#1828=CIRCLE('',#4670,1.65031);
#1829=CIRCLE('',#4672,1.70469);
#1830=CIRCLE('',#4674,1.65031);
#1831=CIRCLE('',#4677,1.70469);
#1832=CIRCLE('',#4678,1.65031);
#1833=CIRCLE('',#4680,1.70469);
#1834=CIRCLE('',#4682,1.65031);
#1835=CIRCLE('',#4691,0.45);
#1836=CIRCLE('',#4693,0.5);
#1837=CIRCLE('',#4695,0.5);
#1838=CIRCLE('',#4697,0.47);
#1839=CIRCLE('',#4699,0.32);
#1840=CIRCLE('',#4701,0.2942);
#1841=CIRCLE('',#4703,0.2942);
#1842=CIRCLE('',#4705,0.24);
#1843=CIRCLE('',#4717,0.3);
#1844=CIRCLE('',#4719,0.35);
#1845=CIRCLE('',#4721,0.35);
#1846=CIRCLE('',#4723,0.32);
#1847=CIRCLE('',#4725,0.22);
#1848=CIRCLE('',#4727,0.1954);
#1849=CIRCLE('',#4729,0.1954);
#1850=CIRCLE('',#4731,0.16);
#1851=CIRCLE('',#4767,1.);
#1852=CIRCLE('',#4771,1.);
#1853=CIRCLE('',#4773,1.2);
#1854=CIRCLE('',#4774,1.);
#1855=CIRCLE('',#4776,1.2);
#1856=CIRCLE('',#4777,1.);
#1857=CIRCLE('',#4780,1.);
#1858=CIRCLE('',#4782,1.);
#1859=CIRCLE('',#4787,1.01);
#1860=CIRCLE('',#4788,1.01);
#1861=CIRCLE('',#4790,1.35);
#1862=CIRCLE('',#4791,1.35);
#1863=CIRCLE('',#4796,0.21);
#1864=CIRCLE('',#4798,0.21);
#1865=CIRCLE('',#4799,0.21);
#1866=CIRCLE('',#4802,1.005);
#1867=CIRCLE('',#4803,1.005);
#1868=CIRCLE('',#4805,1.5);
#1869=CIRCLE('',#4806,1.5);
#1870=CIRCLE('',#4811,0.21);
#1871=CIRCLE('',#4813,0.21);
#1872=CIRCLE('',#4814,0.21);
#1873=CIRCLE('',#4820,1.6);
#1874=CIRCLE('',#4821,1.);
#1875=CIRCLE('',#4823,1.);
#1876=CIRCLE('',#4825,0.33);
#1877=CIRCLE('',#4826,0.33);
#1878=CIRCLE('',#4828,0.33);
#1879=CIRCLE('',#4829,0.33);
#1880=CIRCLE('',#4831,0.33);
#1881=CIRCLE('',#4832,0.33);
#1882=CIRCLE('',#4834,0.33);
#1883=CIRCLE('',#4835,0.33);
#1884=CIRCLE('',#4837,3.5);
#1885=CIRCLE('',#4838,1.6);
#1886=CIRCLE('',#4840,3.5);
#1887=CIRCLE('',#4863,0.22);
#1888=CIRCLE('',#4865,0.24505);
#1889=CIRCLE('',#4867,0.24505);
#1890=CIRCLE('',#4869,0.175);
#1891=VERTEX_POINT('',#6210);
#1892=VERTEX_POINT('',#6212);
#1893=VERTEX_POINT('',#6216);
#1894=VERTEX_POINT('',#6218);
#1895=VERTEX_POINT('',#6222);
#1896=VERTEX_POINT('',#6224);
#1897=VERTEX_POINT('',#6228);
#1898=VERTEX_POINT('',#6230);
#1899=VERTEX_POINT('',#6234);
#1900=VERTEX_POINT('',#6235);
#1901=VERTEX_POINT('',#6237);
#1902=VERTEX_POINT('',#6239);
#1903=VERTEX_POINT('',#6243);
#1904=VERTEX_POINT('',#6245);
#1905=VERTEX_POINT('',#6249);
#1906=VERTEX_POINT('',#6251);
#1907=VERTEX_POINT('',#6261);
#1908=VERTEX_POINT('',#6263);
#1909=VERTEX_POINT('',#6268);
#1910=VERTEX_POINT('',#6270);
#1911=VERTEX_POINT('',#6275);
#1912=VERTEX_POINT('',#6277);
#1913=VERTEX_POINT('',#6282);
#1914=VERTEX_POINT('',#6284);
#1915=VERTEX_POINT('',#6289);
#1916=VERTEX_POINT('',#6291);
#1917=VERTEX_POINT('',#6296);
#1918=VERTEX_POINT('',#6298);
#1919=VERTEX_POINT('',#6303);
#1920=VERTEX_POINT('',#6305);
#1921=VERTEX_POINT('',#6310);
#1922=VERTEX_POINT('',#6312);
#1923=VERTEX_POINT('',#6317);
#1924=VERTEX_POINT('',#6319);
#1925=VERTEX_POINT('',#6323);
#1926=VERTEX_POINT('',#6325);
#1927=VERTEX_POINT('',#6329);
#1928=VERTEX_POINT('',#6331);
#1929=VERTEX_POINT('',#6335);
#1930=VERTEX_POINT('',#6337);
#1931=VERTEX_POINT('',#6341);
#1932=VERTEX_POINT('',#6342);
#1933=VERTEX_POINT('',#6344);
#1934=VERTEX_POINT('',#6346);
#1935=VERTEX_POINT('',#6350);
#1936=VERTEX_POINT('',#6352);
#1937=VERTEX_POINT('',#6354);
#1938=VERTEX_POINT('',#6358);
#1939=VERTEX_POINT('',#6359);
#1940=VERTEX_POINT('',#6361);
#1941=VERTEX_POINT('',#6363);
#1942=VERTEX_POINT('',#6367);
#1943=VERTEX_POINT('',#6369);
#1944=VERTEX_POINT('',#6371);
#1945=VERTEX_POINT('',#6386);
#1946=VERTEX_POINT('',#6387);
#1947=VERTEX_POINT('',#6389);
#1948=VERTEX_POINT('',#6391);
#1949=VERTEX_POINT('',#6395);
#1950=VERTEX_POINT('',#6397);
#1951=VERTEX_POINT('',#6399);
#1952=VERTEX_POINT('',#6403);
#1953=VERTEX_POINT('',#6404);
#1954=VERTEX_POINT('',#6406);
#1955=VERTEX_POINT('',#6408);
#1956=VERTEX_POINT('',#6412);
#1957=VERTEX_POINT('',#6414);
#1958=VERTEX_POINT('',#6416);
#1959=VERTEX_POINT('',#6431);
#1960=VERTEX_POINT('',#6433);
#1961=VERTEX_POINT('',#6437);
#1962=VERTEX_POINT('',#6439);
#1963=VERTEX_POINT('',#6446);
#1964=VERTEX_POINT('',#6448);
#1965=VERTEX_POINT('',#6452);
#1966=VERTEX_POINT('',#6454);
#1967=VERTEX_POINT('',#6461);
#1968=VERTEX_POINT('',#6463);
#1969=VERTEX_POINT('',#6467);
#1970=VERTEX_POINT('',#6469);
#1971=VERTEX_POINT('',#6473);
#1972=VERTEX_POINT('',#6475);
#1973=VERTEX_POINT('',#6479);
#1974=VERTEX_POINT('',#6481);
#1975=VERTEX_POINT('',#6485);
#1976=VERTEX_POINT('',#6487);
#1977=VERTEX_POINT('',#6491);
#1978=VERTEX_POINT('',#6494);
#1979=VERTEX_POINT('',#6496);
#1980=VERTEX_POINT('',#6500);
#1981=VERTEX_POINT('',#6505);
#1982=VERTEX_POINT('',#6507);
#1983=VERTEX_POINT('',#6514);
#1984=VERTEX_POINT('',#6516);
#1985=VERTEX_POINT('',#6520);
#1986=VERTEX_POINT('',#6522);
#1987=VERTEX_POINT('',#6529);
#1988=VERTEX_POINT('',#6531);
#1989=VERTEX_POINT('',#6535);
#1990=VERTEX_POINT('',#6538);
#1991=VERTEX_POINT('',#6540);
#1992=VERTEX_POINT('',#6544);
#1993=VERTEX_POINT('',#6547);
#1994=VERTEX_POINT('',#6549);
#1995=VERTEX_POINT('',#6553);
#1996=VERTEX_POINT('',#6556);
#1997=VERTEX_POINT('',#6558);
#1998=VERTEX_POINT('',#6562);
#1999=VERTEX_POINT('',#6565);
#2000=VERTEX_POINT('',#6569);
#2001=VERTEX_POINT('',#6573);
#2002=VERTEX_POINT('',#6577);
#2003=VERTEX_POINT('',#6581);
#2004=VERTEX_POINT('',#6583);
#2005=VERTEX_POINT('',#6586);
#2006=VERTEX_POINT('',#6590);
#2007=VERTEX_POINT('',#6592);
#2008=VERTEX_POINT('',#6597);
#2009=VERTEX_POINT('',#6602);
#2010=VERTEX_POINT('',#6604);
#2011=VERTEX_POINT('',#6611);
#2012=VERTEX_POINT('',#6612);
#2013=VERTEX_POINT('',#6614);
#2014=VERTEX_POINT('',#6616);
#2015=VERTEX_POINT('',#6620);
#2016=VERTEX_POINT('',#6622);
#2017=VERTEX_POINT('',#6626);
#2018=VERTEX_POINT('',#6628);
#2019=VERTEX_POINT('',#6638);
#2020=VERTEX_POINT('',#6639);
#2021=VERTEX_POINT('',#6641);
#2022=VERTEX_POINT('',#6643);
#2023=VERTEX_POINT('',#6647);
#2024=VERTEX_POINT('',#6649);
#2025=VERTEX_POINT('',#6653);
#2026=VERTEX_POINT('',#6655);
#2027=VERTEX_POINT('',#6666);
#2028=VERTEX_POINT('',#6667);
#2029=VERTEX_POINT('',#6670);
#2030=VERTEX_POINT('',#6672);
#2031=VERTEX_POINT('',#6676);
#2032=VERTEX_POINT('',#6680);
#2033=VERTEX_POINT('',#6682);
#2034=VERTEX_POINT('',#6686);
#2035=VERTEX_POINT('',#6691);
#2036=VERTEX_POINT('',#6695);
#2037=VERTEX_POINT('',#6701);
#2038=VERTEX_POINT('',#6702);
#2039=VERTEX_POINT('',#6705);
#2040=VERTEX_POINT('',#6707);
#2041=VERTEX_POINT('',#6711);
#2042=VERTEX_POINT('',#6715);
#2043=VERTEX_POINT('',#6717);
#2044=VERTEX_POINT('',#6720);
#2045=VERTEX_POINT('',#6724);
#2046=VERTEX_POINT('',#6728);
#2047=VERTEX_POINT('',#6736);
#2048=VERTEX_POINT('',#6737);
#2049=VERTEX_POINT('',#6740);
#2050=VERTEX_POINT('',#6741);
#2051=VERTEX_POINT('',#6744);
#2052=VERTEX_POINT('',#6745);
#2053=VERTEX_POINT('',#6748);
#2054=VERTEX_POINT('',#6749);
#2055=VERTEX_POINT('',#6752);
#2056=VERTEX_POINT('',#6753);
#2057=VERTEX_POINT('',#6756);
#2058=VERTEX_POINT('',#6757);
#2059=VERTEX_POINT('',#6760);
#2060=VERTEX_POINT('',#6761);
#2061=VERTEX_POINT('',#6764);
#2062=VERTEX_POINT('',#6765);
#2063=VERTEX_POINT('',#6769);
#2064=VERTEX_POINT('',#6770);
#2065=VERTEX_POINT('',#6793);
#2066=VERTEX_POINT('',#6795);
#2067=VERTEX_POINT('',#6820);
#2068=VERTEX_POINT('',#6822);
#2069=VERTEX_POINT('',#6845);
#2070=VERTEX_POINT('',#6847);
#2071=VERTEX_POINT('',#6870);
#2072=VERTEX_POINT('',#6872);
#2073=VERTEX_POINT('',#6885);
#2074=VERTEX_POINT('',#6888);
#2075=VERTEX_POINT('',#6901);
#2076=VERTEX_POINT('',#6903);
#2077=VERTEX_POINT('',#6926);
#2078=VERTEX_POINT('',#6928);
#2079=VERTEX_POINT('',#6951);
#2080=VERTEX_POINT('',#6953);
#2081=VERTEX_POINT('',#6976);
#2082=VERTEX_POINT('',#6978);
#2083=VERTEX_POINT('',#7003);
#2084=VERTEX_POINT('',#7007);
#2085=VERTEX_POINT('',#7032);
#2086=VERTEX_POINT('',#7036);
#2087=VERTEX_POINT('',#7061);
#2088=VERTEX_POINT('',#7065);
#2089=VERTEX_POINT('',#7066);
#2090=VERTEX_POINT('',#7093);
#2091=VERTEX_POINT('',#7097);
#2092=VERTEX_POINT('',#7122);
#2093=VERTEX_POINT('',#7126);
#2094=VERTEX_POINT('',#7151);
#2095=VERTEX_POINT('',#7155);
#2096=VERTEX_POINT('',#7180);
#2097=VERTEX_POINT('',#7183);
#2098=VERTEX_POINT('',#7185);
#2099=VERTEX_POINT('',#7217);
#2100=VERTEX_POINT('',#7219);
#2101=VERTEX_POINT('',#7222);
#2102=VERTEX_POINT('',#7226);
#2103=VERTEX_POINT('',#7231);
#2104=VERTEX_POINT('',#7233);
#2105=VERTEX_POINT('',#7236);
#2106=VERTEX_POINT('',#7240);
#2107=VERTEX_POINT('',#7251);
#2108=VERTEX_POINT('',#7254);
#2109=VERTEX_POINT('',#7258);
#2110=VERTEX_POINT('',#7262);
#2111=VERTEX_POINT('',#7266);
#2112=VERTEX_POINT('',#7269);
#2113=VERTEX_POINT('',#7273);
#2114=VERTEX_POINT('',#7277);
#2115=VERTEX_POINT('',#7282);
#2116=VERTEX_POINT('',#7283);
#2117=VERTEX_POINT('',#7285);
#2118=VERTEX_POINT('',#7287);
#2119=VERTEX_POINT('',#7291);
#2120=VERTEX_POINT('',#7293);
#2121=VERTEX_POINT('',#7297);
#2122=VERTEX_POINT('',#7299);
#2123=VERTEX_POINT('',#7303);
#2124=VERTEX_POINT('',#7305);
#2125=VERTEX_POINT('',#7309);
#2126=VERTEX_POINT('',#7311);
#2127=VERTEX_POINT('',#7321);
#2128=VERTEX_POINT('',#7324);
#2129=VERTEX_POINT('',#7328);
#2130=VERTEX_POINT('',#7332);
#2131=VERTEX_POINT('',#7336);
#2132=VERTEX_POINT('',#7339);
#2133=VERTEX_POINT('',#7343);
#2134=VERTEX_POINT('',#7347);
#2135=VERTEX_POINT('',#7352);
#2136=VERTEX_POINT('',#7353);
#2137=VERTEX_POINT('',#7355);
#2138=VERTEX_POINT('',#7357);
#2139=VERTEX_POINT('',#7361);
#2140=VERTEX_POINT('',#7363);
#2141=VERTEX_POINT('',#7367);
#2142=VERTEX_POINT('',#7369);
#2143=VERTEX_POINT('',#7373);
#2144=VERTEX_POINT('',#7375);
#2145=VERTEX_POINT('',#7379);
#2146=VERTEX_POINT('',#7381);
#2147=VERTEX_POINT('',#7414);
#2148=VERTEX_POINT('',#7415);
#2149=VERTEX_POINT('',#7417);
#2150=VERTEX_POINT('',#7419);
#2151=VERTEX_POINT('',#7423);
#2152=VERTEX_POINT('',#7425);
#2153=VERTEX_POINT('',#7429);
#2154=VERTEX_POINT('',#7431);
#2155=VERTEX_POINT('',#7439);
#2156=VERTEX_POINT('',#7441);
#2157=VERTEX_POINT('',#7444);
#2158=VERTEX_POINT('',#7446);
#2159=VERTEX_POINT('',#7451);
#2160=VERTEX_POINT('',#7455);
#2161=VERTEX_POINT('',#7462);
#2162=VERTEX_POINT('',#7464);
#2163=VERTEX_POINT('',#7468);
#2164=VERTEX_POINT('',#7470);
#2165=VERTEX_POINT('',#7477);
#2166=VERTEX_POINT('',#7478);
#2167=VERTEX_POINT('',#7482);
#2168=VERTEX_POINT('',#7497);
#2169=VERTEX_POINT('',#7499);
#2170=VERTEX_POINT('',#7501);
#2171=VERTEX_POINT('',#7538);
#2172=VERTEX_POINT('',#7557);
#2173=VERTEX_POINT('',#7559);
#2174=VERTEX_POINT('',#7563);
#2175=VERTEX_POINT('',#7565);
#2176=VERTEX_POINT('',#7572);
#2177=VERTEX_POINT('',#7573);
#2178=VERTEX_POINT('',#7577);
#2179=VERTEX_POINT('',#7588);
#2180=VERTEX_POINT('',#7590);
#2181=VERTEX_POINT('',#7592);
#2182=VERTEX_POINT('',#7629);
#2183=VERTEX_POINT('',#7644);
#2184=VERTEX_POINT('',#7645);
#2185=VERTEX_POINT('',#7647);
#2186=VERTEX_POINT('',#7649);
#2187=VERTEX_POINT('',#7653);
#2188=VERTEX_POINT('',#7655);
#2189=VERTEX_POINT('',#7659);
#2190=VERTEX_POINT('',#7661);
#2191=VERTEX_POINT('',#7665);
#2192=VERTEX_POINT('',#7671);
#2193=VERTEX_POINT('',#7673);
#2194=VERTEX_POINT('',#7677);
#2195=VERTEX_POINT('',#7679);
#2196=VERTEX_POINT('',#7683);
#2197=VERTEX_POINT('',#7685);
#2198=VERTEX_POINT('',#7689);
#2199=VERTEX_POINT('',#7691);
#2200=VERTEX_POINT('',#7695);
#2201=VERTEX_POINT('',#7697);
#2202=VERTEX_POINT('',#7700);
#2203=VERTEX_POINT('',#7708);
#2204=VERTEX_POINT('',#7709);
#2205=VERTEX_POINT('',#7711);
#2206=VERTEX_POINT('',#7713);
#2207=VERTEX_POINT('',#7715);
#2208=VERTEX_POINT('',#7717);
#2209=VERTEX_POINT('',#7719);
#2210=VERTEX_POINT('',#7721);
#2211=VERTEX_POINT('',#7725);
#2212=VERTEX_POINT('',#7727);
#2213=VERTEX_POINT('',#7731);
#2214=VERTEX_POINT('',#7735);
#2215=VERTEX_POINT('',#7739);
#2216=VERTEX_POINT('',#7743);
#2217=VERTEX_POINT('',#7744);
#2218=VERTEX_POINT('',#7747);
#2219=VERTEX_POINT('',#7759);
#2220=VERTEX_POINT('',#7760);
#2221=VERTEX_POINT('',#7762);
#2222=VERTEX_POINT('',#7764);
#2223=VERTEX_POINT('',#7768);
#2224=VERTEX_POINT('',#7770);
#2225=VERTEX_POINT('',#7774);
#2226=VERTEX_POINT('',#7776);
#2227=VERTEX_POINT('',#7780);
#2228=VERTEX_POINT('',#7782);
#2229=VERTEX_POINT('',#7786);
#2230=VERTEX_POINT('',#7788);
#2231=VERTEX_POINT('',#7796);
#2232=VERTEX_POINT('',#7799);
#2233=VERTEX_POINT('',#7803);
#2234=VERTEX_POINT('',#7807);
#2235=EDGE_CURVE('',#1891,#1891,#1671,.T.);
#2236=EDGE_CURVE('',#1891,#1892,#1147,.T.);
#2237=EDGE_CURVE('',#1892,#1892,#1672,.T.);
#2238=EDGE_CURVE('',#1893,#1893,#1673,.T.);
#2239=EDGE_CURVE('',#1893,#1894,#1148,.T.);
#2240=EDGE_CURVE('',#1894,#1894,#1674,.T.);
#2241=EDGE_CURVE('',#1895,#1895,#1675,.T.);
#2242=EDGE_CURVE('',#1895,#1896,#1149,.T.);
#2243=EDGE_CURVE('',#1896,#1896,#1676,.T.);
#2244=EDGE_CURVE('',#1897,#1897,#1677,.T.);
#2245=EDGE_CURVE('',#1897,#1898,#1150,.T.);
#2246=EDGE_CURVE('',#1898,#1898,#1678,.T.);
#2247=EDGE_CURVE('',#1899,#1900,#1151,.T.);
#2248=EDGE_CURVE('',#1900,#1901,#1152,.T.);
#2249=EDGE_CURVE('',#1902,#1901,#1153,.T.);
#2250=EDGE_CURVE('',#1899,#1902,#1154,.T.);
#2251=EDGE_CURVE('',#1903,#1899,#1155,.T.);
#2252=EDGE_CURVE('',#1904,#1902,#1156,.T.);
#2253=EDGE_CURVE('',#1903,#1904,#1157,.T.);
#2254=EDGE_CURVE('',#1905,#1903,#1158,.T.);
#2255=EDGE_CURVE('',#1906,#1904,#1159,.T.);
#2256=EDGE_CURVE('',#1905,#1906,#1160,.T.);
#2257=EDGE_CURVE('',#1900,#1905,#1161,.T.);
#2258=EDGE_CURVE('',#1901,#1906,#1162,.T.);
#2259=EDGE_CURVE('',#1907,#1907,#1679,.T.);
#2260=EDGE_CURVE('',#1907,#1908,#1163,.T.);
#2261=EDGE_CURVE('',#1908,#1908,#1680,.T.);
#2262=EDGE_CURVE('',#1909,#1909,#1681,.T.);
#2263=EDGE_CURVE('',#1909,#1910,#1164,.T.);
#2264=EDGE_CURVE('',#1910,#1910,#1682,.T.);
#2265=EDGE_CURVE('',#1911,#1911,#1683,.T.);
#2266=EDGE_CURVE('',#1911,#1912,#1165,.T.);
#2267=EDGE_CURVE('',#1912,#1912,#1684,.T.);
#2268=EDGE_CURVE('',#1913,#1913,#1685,.T.);
#2269=EDGE_CURVE('',#1913,#1914,#1166,.T.);
#2270=EDGE_CURVE('',#1914,#1914,#1686,.T.);
#2271=EDGE_CURVE('',#1915,#1915,#1687,.T.);
#2272=EDGE_CURVE('',#1915,#1916,#1167,.T.);
#2273=EDGE_CURVE('',#1916,#1916,#1688,.T.);
#2274=EDGE_CURVE('',#1917,#1917,#1689,.T.);
#2275=EDGE_CURVE('',#1917,#1918,#1168,.T.);
#2276=EDGE_CURVE('',#1918,#1918,#1690,.T.);
#2277=EDGE_CURVE('',#1919,#1919,#1691,.T.);
#2278=EDGE_CURVE('',#1919,#1920,#1169,.T.);
#2279=EDGE_CURVE('',#1920,#1920,#1692,.T.);
#2280=EDGE_CURVE('',#1921,#1921,#1693,.T.);
#2281=EDGE_CURVE('',#1921,#1922,#1170,.T.);
#2282=EDGE_CURVE('',#1922,#1922,#1694,.T.);
#2283=EDGE_CURVE('',#1923,#1923,#1695,.T.);
#2284=EDGE_CURVE('',#1923,#1924,#1171,.T.);
#2285=EDGE_CURVE('',#1924,#1924,#1696,.T.);
#2286=EDGE_CURVE('',#1925,#1925,#1697,.T.);
#2287=EDGE_CURVE('',#1925,#1926,#1172,.T.);
#2288=EDGE_CURVE('',#1926,#1926,#1698,.T.);
#2289=EDGE_CURVE('',#1927,#1927,#1699,.T.);
#2290=EDGE_CURVE('',#1927,#1928,#1173,.T.);
#2291=EDGE_CURVE('',#1928,#1928,#1700,.T.);
#2292=EDGE_CURVE('',#1929,#1929,#1701,.T.);
#2293=EDGE_CURVE('',#1929,#1930,#1174,.T.);
#2294=EDGE_CURVE('',#1930,#1930,#1702,.T.);
#2295=EDGE_CURVE('',#1931,#1932,#1703,.T.);
#2296=EDGE_CURVE('',#1931,#1933,#1175,.T.);
#2297=EDGE_CURVE('',#1933,#1934,#1176,.T.);
#2298=EDGE_CURVE('',#1934,#1932,#1177,.T.);
#2299=EDGE_CURVE('',#1932,#1935,#1704,.T.);
#2300=EDGE_CURVE('',#1932,#1936,#1178,.T.);
#2301=EDGE_CURVE('',#1936,#1937,#1179,.T.);
#2302=EDGE_CURVE('',#1937,#1935,#1180,.T.);
#2303=EDGE_CURVE('',#1938,#1939,#1705,.T.);
#2304=EDGE_CURVE('',#1938,#1940,#1181,.T.);
#2305=EDGE_CURVE('',#1940,#1941,#1182,.T.);
#2306=EDGE_CURVE('',#1941,#1939,#1183,.T.);
#2307=EDGE_CURVE('',#1942,#1938,#1706,.T.);
#2308=EDGE_CURVE('',#1942,#1943,#1184,.T.);
#2309=EDGE_CURVE('',#1943,#1944,#1185,.T.);
#2310=EDGE_CURVE('',#1944,#1938,#1186,.T.);
#2311=EDGE_CURVE('',#1939,#1931,#1187,.T.);
#2312=EDGE_CURVE('',#1941,#1933,#1188,.T.);
#2313=EDGE_CURVE('',#1935,#1942,#1189,.T.);
#2314=EDGE_CURVE('',#1943,#1937,#1190,.T.);
#2315=EDGE_CURVE('',#1944,#1936,#1191,.T.);
#2316=EDGE_CURVE('',#1940,#1934,#1192,.T.);
#2317=EDGE_CURVE('',#1945,#1946,#1707,.T.);
#2318=EDGE_CURVE('',#1945,#1947,#1193,.T.);
#2319=EDGE_CURVE('',#1947,#1948,#1194,.T.);
#2320=EDGE_CURVE('',#1948,#1946,#1195,.T.);
#2321=EDGE_CURVE('',#1946,#1949,#1708,.T.);
#2322=EDGE_CURVE('',#1946,#1950,#1196,.T.);
#2323=EDGE_CURVE('',#1950,#1951,#1197,.T.);
#2324=EDGE_CURVE('',#1951,#1949,#1198,.T.);
#2325=EDGE_CURVE('',#1952,#1953,#1709,.T.);
#2326=EDGE_CURVE('',#1952,#1954,#1199,.T.);
#2327=EDGE_CURVE('',#1954,#1955,#1200,.T.);
#2328=EDGE_CURVE('',#1955,#1953,#1201,.T.);
#2329=EDGE_CURVE('',#1956,#1952,#1710,.T.);
#2330=EDGE_CURVE('',#1956,#1957,#1202,.T.);
#2331=EDGE_CURVE('',#1957,#1958,#1203,.T.);
#2332=EDGE_CURVE('',#1958,#1952,#1204,.T.);
#2333=EDGE_CURVE('',#1953,#1945,#1205,.T.);
#2334=EDGE_CURVE('',#1955,#1947,#1206,.T.);
#2335=EDGE_CURVE('',#1949,#1956,#1207,.T.);
#2336=EDGE_CURVE('',#1957,#1951,#1208,.T.);
#2337=EDGE_CURVE('',#1958,#1950,#1209,.T.);
#2338=EDGE_CURVE('',#1954,#1948,#1210,.T.);
#2339=EDGE_CURVE('',#1959,#1959,#1711,.T.);
#2340=EDGE_CURVE('',#1959,#1960,#1211,.T.);
#2341=EDGE_CURVE('',#1960,#1960,#1712,.T.);
#2342=EDGE_CURVE('',#1961,#1961,#1713,.T.);
#2343=EDGE_CURVE('',#1961,#1962,#1212,.T.);
#2344=EDGE_CURVE('',#1962,#1962,#1714,.T.);
#2345=EDGE_CURVE('',#1963,#1963,#1715,.T.);
#2346=EDGE_CURVE('',#1963,#1964,#1213,.T.);
#2347=EDGE_CURVE('',#1964,#1964,#1716,.T.);
#2348=EDGE_CURVE('',#1965,#1965,#1717,.T.);
#2349=EDGE_CURVE('',#1965,#1966,#1214,.T.);
#2350=EDGE_CURVE('',#1966,#1966,#1718,.T.);
#2351=EDGE_CURVE('',#1967,#1967,#1719,.T.);
#2352=EDGE_CURVE('',#1967,#1968,#1215,.T.);
#2353=EDGE_CURVE('',#1968,#1968,#1720,.T.);
#2354=EDGE_CURVE('',#1969,#1969,#1721,.T.);
#2355=EDGE_CURVE('',#1969,#1970,#1216,.T.);
#2356=EDGE_CURVE('',#1970,#1970,#1722,.T.);
#2357=EDGE_CURVE('',#1971,#1971,#1723,.T.);
#2358=EDGE_CURVE('',#1971,#1972,#1217,.T.);
#2359=EDGE_CURVE('',#1972,#1972,#1724,.T.);
#2360=EDGE_CURVE('',#1973,#1973,#1725,.T.);
#2361=EDGE_CURVE('',#1973,#1974,#1218,.T.);
#2362=EDGE_CURVE('',#1974,#1974,#1726,.T.);
#2363=EDGE_CURVE('',#1975,#1975,#1727,.T.);
#2364=EDGE_CURVE('',#1975,#1976,#1219,.T.);
#2365=EDGE_CURVE('',#1976,#1976,#1728,.T.);
#2366=EDGE_CURVE('',#1977,#1977,#1729,.T.);
#2367=EDGE_CURVE('',#1978,#1978,#1730,.T.);
#2368=EDGE_CURVE('',#1978,#1979,#1220,.T.);
#2369=EDGE_CURVE('',#1979,#1979,#1731,.T.);
#2370=EDGE_CURVE('',#1980,#1980,#1732,.T.);
#2371=EDGE_CURVE('',#1977,#1980,#1221,.T.);
#2372=EDGE_CURVE('',#1981,#1981,#1733,.T.);
#2373=EDGE_CURVE('',#1981,#1982,#1222,.T.);
#2374=EDGE_CURVE('',#1982,#1982,#1734,.T.);
#2375=EDGE_CURVE('',#1983,#1983,#1735,.T.);
#2376=EDGE_CURVE('',#1983,#1984,#1223,.T.);
#2377=EDGE_CURVE('',#1984,#1984,#1736,.T.);
#2378=EDGE_CURVE('',#1985,#1985,#1737,.T.);
#2379=EDGE_CURVE('',#1985,#1986,#1224,.T.);
#2380=EDGE_CURVE('',#1986,#1986,#1738,.T.);
#2381=EDGE_CURVE('',#1987,#1987,#1739,.T.);
#2382=EDGE_CURVE('',#1987,#1988,#1225,.T.);
#2383=EDGE_CURVE('',#1988,#1988,#1740,.T.);
#2384=EDGE_CURVE('',#1989,#1989,#1741,.T.);
#2385=EDGE_CURVE('',#1990,#1990,#1742,.T.);
#2386=EDGE_CURVE('',#1990,#1991,#1226,.T.);
#2387=EDGE_CURVE('',#1991,#1991,#1743,.T.);
#2388=EDGE_CURVE('',#1992,#1992,#1744,.T.);
#2389=EDGE_CURVE('',#1993,#1993,#1745,.T.);
#2390=EDGE_CURVE('',#1993,#1994,#1227,.T.);
#2391=EDGE_CURVE('',#1994,#1994,#1746,.T.);
#2392=EDGE_CURVE('',#1995,#1995,#1747,.T.);
#2393=EDGE_CURVE('',#1996,#1996,#1748,.T.);
#2394=EDGE_CURVE('',#1996,#1997,#1228,.T.);
#2395=EDGE_CURVE('',#1997,#1997,#1749,.T.);
#2396=EDGE_CURVE('',#1998,#1998,#1750,.T.);
#2397=EDGE_CURVE('',#1999,#1999,#1751,.T.);
#2398=EDGE_CURVE('',#1999,#1989,#1229,.T.);
#2399=EDGE_CURVE('',#2000,#2000,#1752,.T.);
#2400=EDGE_CURVE('',#2000,#1992,#1230,.T.);
#2401=EDGE_CURVE('',#2001,#2001,#1753,.T.);
#2402=EDGE_CURVE('',#2001,#1995,#1231,.T.);
#2403=EDGE_CURVE('',#2002,#2002,#1754,.T.);
#2404=EDGE_CURVE('',#2002,#1998,#1232,.T.);
#2405=EDGE_CURVE('',#2003,#2003,#1755,.T.);
#2406=EDGE_CURVE('',#2004,#2004,#1756,.T.);
#2407=EDGE_CURVE('',#2004,#2005,#1233,.T.);
#2408=EDGE_CURVE('',#2005,#2005,#1757,.T.);
#2409=EDGE_CURVE('',#2006,#2006,#1758,.T.);
#2410=EDGE_CURVE('',#2006,#2007,#1234,.T.);
#2411=EDGE_CURVE('',#2007,#2007,#1759,.T.);
#2412=EDGE_CURVE('',#2003,#2008,#1235,.T.);
#2413=EDGE_CURVE('',#2008,#2008,#1760,.T.);
#2414=EDGE_CURVE('',#2009,#2009,#1761,.T.);
#2415=EDGE_CURVE('',#2009,#2010,#1236,.T.);
#2416=EDGE_CURVE('',#2010,#2010,#1762,.T.);
#2417=EDGE_CURVE('',#2011,#2012,#1237,.T.);
#2418=EDGE_CURVE('',#2012,#2013,#1238,.T.);
#2419=EDGE_CURVE('',#2014,#2013,#1239,.T.);
#2420=EDGE_CURVE('',#2011,#2014,#1240,.T.);
#2421=EDGE_CURVE('',#2015,#2011,#1241,.T.);
#2422=EDGE_CURVE('',#2016,#2014,#1242,.T.);
#2423=EDGE_CURVE('',#2015,#2016,#1243,.T.);
#2424=EDGE_CURVE('',#2017,#2015,#1244,.T.);
#2425=EDGE_CURVE('',#2018,#2016,#1245,.T.);
#2426=EDGE_CURVE('',#2017,#2018,#1246,.T.);
#2427=EDGE_CURVE('',#2012,#2017,#1247,.T.);
#2428=EDGE_CURVE('',#2013,#2018,#1248,.T.);
#2429=EDGE_CURVE('',#2019,#2020,#1249,.T.);
#2430=EDGE_CURVE('',#2020,#2021,#1250,.T.);
#2431=EDGE_CURVE('',#2022,#2021,#1251,.T.);
#2432=EDGE_CURVE('',#2019,#2022,#1252,.T.);
#2433=EDGE_CURVE('',#2023,#2019,#1253,.T.);
#2434=EDGE_CURVE('',#2024,#2022,#1254,.T.);
#2435=EDGE_CURVE('',#2023,#2024,#1255,.T.);
#2436=EDGE_CURVE('',#2025,#2023,#1256,.T.);
#2437=EDGE_CURVE('',#2026,#2024,#1257,.T.);
#2438=EDGE_CURVE('',#2025,#2026,#1258,.T.);
#2439=EDGE_CURVE('',#2020,#2025,#1259,.T.);
#2440=EDGE_CURVE('',#2021,#2026,#1260,.T.);
#2441=EDGE_CURVE('',#2027,#2028,#1763,.T.);
#2442=EDGE_CURVE('',#2028,#2027,#1764,.T.);
#2443=EDGE_CURVE('',#2028,#2029,#1765,.T.);
#2444=EDGE_CURVE('',#2030,#2029,#1766,.T.);
#2445=EDGE_CURVE('',#2029,#2030,#1767,.T.);
#2446=EDGE_CURVE('',#2030,#2031,#1261,.T.);
#2447=EDGE_CURVE('',#2031,#2031,#1768,.T.);
#2448=EDGE_CURVE('',#2032,#2032,#1769,.T.);
#2449=EDGE_CURVE('',#2032,#2033,#1262,.T.);
#2450=EDGE_CURVE('',#2033,#2033,#1770,.T.);
#2451=EDGE_CURVE('',#2033,#2034,#1263,.T.);
#2452=EDGE_CURVE('',#2034,#2034,#1771,.T.);
#2453=EDGE_CURVE('',#2035,#2035,#1772,.T.);
#2454=EDGE_CURVE('',#2035,#2027,#1264,.T.);
#2455=EDGE_CURVE('',#2036,#2036,#1773,.T.);
#2456=EDGE_CURVE('',#2036,#2032,#1265,.T.);
#2457=EDGE_CURVE('',#2037,#2038,#1774,.T.);
#2458=EDGE_CURVE('',#2038,#2037,#1775,.T.);
#2459=EDGE_CURVE('',#2038,#2039,#1776,.T.);
#2460=EDGE_CURVE('',#2040,#2039,#1777,.T.);
#2461=EDGE_CURVE('',#2039,#2040,#1778,.T.);
#2462=EDGE_CURVE('',#2041,#2041,#1779,.T.);
#2463=EDGE_CURVE('',#2041,#2040,#1266,.T.);
#2464=EDGE_CURVE('',#2042,#2042,#1780,.T.);
#2465=EDGE_CURVE('',#2043,#2043,#1781,.T.);
#2466=EDGE_CURVE('',#2044,#2044,#1782,.T.);
#2467=EDGE_CURVE('',#2044,#2042,#1267,.T.);
#2468=EDGE_CURVE('',#2045,#2045,#1783,.T.);
#2469=EDGE_CURVE('',#2045,#2044,#1268,.T.);
#2470=EDGE_CURVE('',#2046,#2046,#1784,.T.);
#2471=EDGE_CURVE('',#2046,#2045,#1269,.T.);
#2472=EDGE_CURVE('',#2037,#2043,#1270,.T.);
#2473=EDGE_CURVE('',#2047,#2048,#1785,.T.);
#2474=EDGE_CURVE('',#2049,#2050,#1786,.T.);
#2475=EDGE_CURVE('',#2051,#2052,#1787,.T.);
#2476=EDGE_CURVE('',#2053,#2054,#1788,.T.);
#2477=EDGE_CURVE('',#2055,#2056,#1789,.T.);
#2478=EDGE_CURVE('',#2057,#2058,#1790,.T.);
#2479=EDGE_CURVE('',#2059,#2060,#1791,.T.);
#2480=EDGE_CURVE('',#2061,#2062,#1792,.T.);
#2481=EDGE_CURVE('',#2063,#2064,#159,.T.);
#2482=EDGE_CURVE('',#2065,#2063,#1793,.T.);
#2483=EDGE_CURVE('',#2066,#2065,#160,.T.);
#2484=EDGE_CURVE('',#2064,#2066,#1794,.T.);
#2485=EDGE_CURVE('',#2067,#2065,#1795,.T.);
#2486=EDGE_CURVE('',#2067,#2068,#161,.T.);
#2487=EDGE_CURVE('',#2069,#2068,#1796,.T.);
#2488=EDGE_CURVE('',#2069,#2070,#162,.T.);
#2489=EDGE_CURVE('',#2071,#2070,#1797,.T.);
#2490=EDGE_CURVE('',#2071,#2072,#163,.T.);
#2491=EDGE_CURVE('',#2072,#2073,#1271,.T.);
#2492=EDGE_CURVE('',#2073,#2073,#1798,.T.);
#2493=EDGE_CURVE('',#2072,#2074,#164,.T.);
#2494=EDGE_CURVE('',#2075,#2074,#1799,.T.);
#2495=EDGE_CURVE('',#2075,#2076,#165,.T.);
#2496=EDGE_CURVE('',#2077,#2076,#1800,.T.);
#2497=EDGE_CURVE('',#2077,#2078,#166,.T.);
#2498=EDGE_CURVE('',#2079,#2078,#1801,.T.);
#2499=EDGE_CURVE('',#2079,#2080,#167,.T.);
#2500=EDGE_CURVE('',#2081,#2080,#1802,.T.);
#2501=EDGE_CURVE('',#2081,#2082,#168,.T.);
#2502=EDGE_CURVE('',#2066,#2082,#1803,.T.);
#2503=EDGE_CURVE('',#2063,#2083,#1804,.T.);
#2504=EDGE_CURVE('',#2083,#2067,#1805,.T.);
#2505=EDGE_CURVE('',#2084,#2083,#169,.T.);
#2506=EDGE_CURVE('',#2068,#2084,#1806,.T.);
#2507=EDGE_CURVE('',#2084,#2085,#1807,.T.);
#2508=EDGE_CURVE('',#2085,#2069,#1808,.T.);
#2509=EDGE_CURVE('',#2086,#2085,#170,.T.);
#2510=EDGE_CURVE('',#2070,#2086,#1809,.T.);
#2511=EDGE_CURVE('',#2086,#2087,#1810,.T.);
#2512=EDGE_CURVE('',#2087,#2071,#1811,.T.);
#2513=EDGE_CURVE('',#2088,#2089,#171,.T.);
#2514=EDGE_CURVE('',#2074,#2088,#1812,.T.);
#2515=EDGE_CURVE('',#2089,#2087,#172,.T.);
#2516=EDGE_CURVE('',#2088,#2090,#1813,.T.);
#2517=EDGE_CURVE('',#2090,#2075,#1814,.T.);
#2518=EDGE_CURVE('',#2091,#2090,#173,.T.);
#2519=EDGE_CURVE('',#2076,#2091,#1815,.T.);
#2520=EDGE_CURVE('',#2091,#2092,#1816,.T.);
#2521=EDGE_CURVE('',#2092,#2077,#1817,.T.);
#2522=EDGE_CURVE('',#2093,#2092,#174,.T.);
#2523=EDGE_CURVE('',#2078,#2093,#1818,.T.);
#2524=EDGE_CURVE('',#2093,#2094,#1819,.T.);
#2525=EDGE_CURVE('',#2094,#2079,#1820,.T.);
#2526=EDGE_CURVE('',#2095,#2094,#175,.T.);
#2527=EDGE_CURVE('',#2080,#2095,#1821,.T.);
#2528=EDGE_CURVE('',#2096,#2096,#1822,.T.);
#2529=EDGE_CURVE('',#2096,#2089,#1272,.T.);
#2530=EDGE_CURVE('',#2097,#2064,#1823,.T.);
#2531=EDGE_CURVE('',#2097,#2098,#176,.T.);
#2532=EDGE_CURVE('',#2095,#2098,#1824,.T.);
#2533=EDGE_CURVE('',#2082,#2097,#1825,.T.);
#2534=EDGE_CURVE('',#2098,#2081,#1826,.T.);
#2535=EDGE_CURVE('',#2099,#2099,#1827,.T.);
#2536=EDGE_CURVE('',#2100,#2100,#1828,.T.);
#2537=EDGE_CURVE('',#2101,#2101,#1829,.T.);
#2538=EDGE_CURVE('',#2101,#2099,#1273,.T.);
#2539=EDGE_CURVE('',#2102,#2102,#1830,.T.);
#2540=EDGE_CURVE('',#2102,#2100,#1274,.T.);
#2541=EDGE_CURVE('',#2103,#2103,#1831,.T.);
#2542=EDGE_CURVE('',#2104,#2104,#1832,.T.);
#2543=EDGE_CURVE('',#2105,#2105,#1833,.T.);
#2544=EDGE_CURVE('',#2105,#2103,#1275,.T.);
#2545=EDGE_CURVE('',#2106,#2106,#1834,.T.);
#2546=EDGE_CURVE('',#2106,#2104,#1276,.T.);
#2547=EDGE_CURVE('',#2107,#2107,#1835,.T.);
#2548=EDGE_CURVE('',#2108,#2108,#1836,.T.);
#2549=EDGE_CURVE('',#2108,#2107,#1277,.T.);
#2550=EDGE_CURVE('',#2109,#2109,#1837,.T.);
#2551=EDGE_CURVE('',#2109,#2108,#1278,.T.);
#2552=EDGE_CURVE('',#2110,#2110,#1838,.T.);
#2553=EDGE_CURVE('',#2110,#2109,#1279,.T.);
#2554=EDGE_CURVE('',#2111,#2111,#1839,.T.);
#2555=EDGE_CURVE('',#2112,#2112,#1840,.F.);
#2556=EDGE_CURVE('',#2112,#2111,#1280,.T.);
#2557=EDGE_CURVE('',#2113,#2113,#1841,.F.);
#2558=EDGE_CURVE('',#2113,#2112,#1281,.T.);
#2559=EDGE_CURVE('',#2114,#2114,#1842,.T.);
#2560=EDGE_CURVE('',#2114,#2113,#1282,.T.);
#2561=EDGE_CURVE('',#2115,#2116,#1283,.T.);
#2562=EDGE_CURVE('',#2116,#2117,#1284,.T.);
#2563=EDGE_CURVE('',#2117,#2118,#1285,.T.);
#2564=EDGE_CURVE('',#2115,#2118,#1286,.T.);
#2565=EDGE_CURVE('',#2116,#2119,#1287,.T.);
#2566=EDGE_CURVE('',#2119,#2120,#1288,.T.);
#2567=EDGE_CURVE('',#2120,#2117,#1289,.T.);
#2568=EDGE_CURVE('',#2119,#2121,#1290,.T.);
#2569=EDGE_CURVE('',#2121,#2122,#1291,.T.);
#2570=EDGE_CURVE('',#2122,#2120,#1292,.T.);
#2571=EDGE_CURVE('',#2121,#2123,#1293,.T.);
#2572=EDGE_CURVE('',#2123,#2124,#1294,.T.);
#2573=EDGE_CURVE('',#2124,#2122,#1295,.T.);
#2574=EDGE_CURVE('',#2123,#2125,#1296,.T.);
#2575=EDGE_CURVE('',#2125,#2126,#1297,.T.);
#2576=EDGE_CURVE('',#2126,#2124,#1298,.T.);
#2577=EDGE_CURVE('',#2125,#2115,#1299,.T.);
#2578=EDGE_CURVE('',#2118,#2126,#1300,.T.);
#2579=EDGE_CURVE('',#2127,#2127,#1843,.T.);
#2580=EDGE_CURVE('',#2128,#2128,#1844,.T.);
#2581=EDGE_CURVE('',#2128,#2127,#1301,.T.);
#2582=EDGE_CURVE('',#2129,#2129,#1845,.T.);
#2583=EDGE_CURVE('',#2129,#2128,#1302,.T.);
#2584=EDGE_CURVE('',#2130,#2130,#1846,.T.);
#2585=EDGE_CURVE('',#2130,#2129,#1303,.T.);
#2586=EDGE_CURVE('',#2131,#2131,#1847,.T.);
#2587=EDGE_CURVE('',#2132,#2132,#1848,.F.);
#2588=EDGE_CURVE('',#2132,#2131,#1304,.T.);
#2589=EDGE_CURVE('',#2133,#2133,#1849,.F.);
#2590=EDGE_CURVE('',#2133,#2132,#1305,.T.);
#2591=EDGE_CURVE('',#2134,#2134,#1850,.T.);
#2592=EDGE_CURVE('',#2134,#2133,#1306,.T.);
#2593=EDGE_CURVE('',#2135,#2136,#1307,.T.);
#2594=EDGE_CURVE('',#2136,#2137,#1308,.T.);
#2595=EDGE_CURVE('',#2137,#2138,#1309,.T.);
#2596=EDGE_CURVE('',#2135,#2138,#1310,.T.);
#2597=EDGE_CURVE('',#2136,#2139,#1311,.T.);
#2598=EDGE_CURVE('',#2139,#2140,#1312,.T.);
#2599=EDGE_CURVE('',#2140,#2137,#1313,.T.);
#2600=EDGE_CURVE('',#2139,#2141,#1314,.T.);
#2601=EDGE_CURVE('',#2141,#2142,#1315,.T.);
#2602=EDGE_CURVE('',#2142,#2140,#1316,.T.);
#2603=EDGE_CURVE('',#2141,#2143,#1317,.T.);
#2604=EDGE_CURVE('',#2143,#2144,#1318,.T.);
#2605=EDGE_CURVE('',#2144,#2142,#1319,.T.);
#2606=EDGE_CURVE('',#2143,#2145,#1320,.T.);
#2607=EDGE_CURVE('',#2145,#2146,#1321,.T.);
#2608=EDGE_CURVE('',#2146,#2144,#1322,.T.);
#2609=EDGE_CURVE('',#2145,#2135,#1323,.T.);
#2610=EDGE_CURVE('',#2138,#2146,#1324,.T.);
#2611=EDGE_CURVE('',#2147,#2148,#1325,.T.);
#2612=EDGE_CURVE('',#2147,#2149,#1326,.T.);
#2613=EDGE_CURVE('',#2150,#2149,#1327,.T.);
#2614=EDGE_CURVE('',#2150,#2148,#1328,.T.);
#2615=EDGE_CURVE('',#2148,#2151,#1851,.T.);
#2616=EDGE_CURVE('',#2152,#2150,#1329,.T.);
#2617=EDGE_CURVE('',#2151,#2152,#1330,.T.);
#2618=EDGE_CURVE('',#2151,#2153,#1331,.T.);
#2619=EDGE_CURVE('',#2152,#2154,#1332,.T.);
#2620=EDGE_CURVE('',#2154,#2153,#1333,.T.);
#2621=EDGE_CURVE('',#2149,#2154,#1334,.T.);
#2622=EDGE_CURVE('',#2153,#2147,#1852,.T.);
#2623=EDGE_CURVE('',#2155,#2155,#1853,.T.);
#2624=EDGE_CURVE('',#2156,#2156,#1854,.T.);
#2625=EDGE_CURVE('',#2157,#2157,#1855,.T.);
#2626=EDGE_CURVE('',#2158,#2158,#1856,.T.);
#2627=EDGE_CURVE('',#2155,#2157,#1335,.T.);
#2628=EDGE_CURVE('',#2158,#2159,#1336,.T.);
#2629=EDGE_CURVE('',#2159,#2159,#1857,.T.);
#2630=EDGE_CURVE('',#2160,#2160,#1858,.T.);
#2631=EDGE_CURVE('',#2160,#2156,#1337,.T.);
#2632=EDGE_CURVE('',#2161,#2161,#1859,.T.);
#2633=EDGE_CURVE('',#2161,#2162,#1338,.T.);
#2634=EDGE_CURVE('',#2162,#2162,#1860,.T.);
#2635=EDGE_CURVE('',#2163,#2163,#1861,.T.);
#2636=EDGE_CURVE('',#2163,#2164,#1339,.T.);
#2637=EDGE_CURVE('',#2164,#2164,#1862,.T.);
#2638=EDGE_CURVE('',#2165,#2166,#1340,.T.);
#2639=EDGE_CURVE('',#2165,#2166,#1863,.T.);
#2640=EDGE_CURVE('',#2167,#2165,#177,.T.);
#2641=EDGE_CURVE('',#2168,#2167,#1864,.T.);
#2642=EDGE_CURVE('',#2168,#2169,#1341,.T.);
#2643=EDGE_CURVE('',#2170,#2169,#178,.T.);
#2644=EDGE_CURVE('',#2169,#2170,#179,.T.);
#2645=EDGE_CURVE('',#2171,#2168,#1865,.T.);
#2646=EDGE_CURVE('',#2166,#2171,#180,.T.);
#2647=EDGE_CURVE('',#2171,#2167,#1342,.T.);
#2648=EDGE_CURVE('',#2172,#2172,#1866,.T.);
#2649=EDGE_CURVE('',#2172,#2173,#1343,.T.);
#2650=EDGE_CURVE('',#2173,#2173,#1867,.T.);
#2651=EDGE_CURVE('',#2174,#2174,#1868,.T.);
#2652=EDGE_CURVE('',#2174,#2175,#1344,.T.);
#2653=EDGE_CURVE('',#2175,#2175,#1869,.T.);
#2654=EDGE_CURVE('',#2176,#2177,#1345,.T.);
#2655=EDGE_CURVE('',#2176,#2177,#1870,.T.);
#2656=EDGE_CURVE('',#2178,#2176,#181,.T.);
#2657=EDGE_CURVE('',#2179,#2178,#1871,.T.);
#2658=EDGE_CURVE('',#2179,#2180,#1346,.T.);
#2659=EDGE_CURVE('',#2181,#2180,#182,.T.);
#2660=EDGE_CURVE('',#2180,#2181,#183,.T.);
#2661=EDGE_CURVE('',#2182,#2179,#1872,.T.);
#2662=EDGE_CURVE('',#2177,#2182,#184,.T.);
#2663=EDGE_CURVE('',#2182,#2178,#1347,.T.);
#2664=EDGE_CURVE('',#2183,#2184,#1348,.T.);
#2665=EDGE_CURVE('',#2183,#2185,#1349,.T.);
#2666=EDGE_CURVE('',#2186,#2185,#1350,.T.);
#2667=EDGE_CURVE('',#2184,#2186,#1351,.T.);
#2668=EDGE_CURVE('',#2187,#2183,#1352,.T.);
#2669=EDGE_CURVE('',#2187,#2188,#1353,.T.);
#2670=EDGE_CURVE('',#2185,#2188,#1354,.T.);
#2671=EDGE_CURVE('',#2189,#2187,#1355,.T.);
#2672=EDGE_CURVE('',#2190,#2189,#1356,.T.);
#2673=EDGE_CURVE('',#2188,#2190,#1357,.T.);
#2674=EDGE_CURVE('',#2191,#2191,#1873,.T.);
#2675=EDGE_CURVE('',#2190,#2186,#1874,.T.);
#2676=EDGE_CURVE('',#2189,#2184,#1875,.T.);
#2677=EDGE_CURVE('',#2192,#2192,#1876,.T.);
#2678=EDGE_CURVE('',#2192,#2193,#1358,.T.);
#2679=EDGE_CURVE('',#2193,#2193,#1877,.T.);
#2680=EDGE_CURVE('',#2194,#2194,#1878,.T.);
#2681=EDGE_CURVE('',#2194,#2195,#1359,.T.);
#2682=EDGE_CURVE('',#2195,#2195,#1879,.T.);
#2683=EDGE_CURVE('',#2196,#2196,#1880,.T.);
#2684=EDGE_CURVE('',#2196,#2197,#1360,.T.);
#2685=EDGE_CURVE('',#2197,#2197,#1881,.T.);
#2686=EDGE_CURVE('',#2198,#2198,#1882,.T.);
#2687=EDGE_CURVE('',#2198,#2199,#1361,.T.);
#2688=EDGE_CURVE('',#2199,#2199,#1883,.T.);
#2689=EDGE_CURVE('',#2200,#2200,#1884,.T.);
#2690=EDGE_CURVE('',#2201,#2201,#1885,.T.);
#2691=EDGE_CURVE('',#2200,#2202,#1362,.T.);
#2692=EDGE_CURVE('',#2202,#2202,#1886,.T.);
#2693=EDGE_CURVE('',#2191,#2201,#1363,.T.);
#2694=EDGE_CURVE('',#2203,#2204,#1364,.T.);
#2695=EDGE_CURVE('',#2205,#2203,#1365,.T.);
#2696=EDGE_CURVE('',#2206,#2205,#1366,.T.);
#2697=EDGE_CURVE('',#2207,#2206,#1367,.T.);
#2698=EDGE_CURVE('',#2208,#2207,#1368,.T.);
#2699=EDGE_CURVE('',#2209,#2208,#1369,.T.);
#2700=EDGE_CURVE('',#2210,#2209,#1370,.T.);
#2701=EDGE_CURVE('',#2204,#2210,#1371,.T.);
#2702=EDGE_CURVE('',#2207,#2211,#1372,.T.);
#2703=EDGE_CURVE('',#2211,#2212,#1373,.T.);
#2704=EDGE_CURVE('',#2212,#2208,#1374,.T.);
#2705=EDGE_CURVE('',#2213,#2206,#1375,.T.);
#2706=EDGE_CURVE('',#2213,#2211,#1376,.T.);
#2707=EDGE_CURVE('',#2205,#2214,#1377,.T.);
#2708=EDGE_CURVE('',#2214,#2213,#1378,.T.);
#2709=EDGE_CURVE('',#2215,#2203,#1379,.T.);
#2710=EDGE_CURVE('',#2215,#2214,#1380,.T.);
#2711=EDGE_CURVE('',#2216,#2217,#1381,.T.);
#2712=EDGE_CURVE('',#2212,#2216,#1382,.T.);
#2713=EDGE_CURVE('',#2218,#2215,#1383,.T.);
#2714=EDGE_CURVE('',#2217,#2218,#1384,.T.);
#2715=EDGE_CURVE('',#2209,#2216,#1385,.T.);
#2716=EDGE_CURVE('',#2204,#2218,#1386,.T.);
#2717=EDGE_CURVE('',#2217,#2210,#1387,.T.);
#2718=EDGE_CURVE('',#2219,#2220,#1388,.T.);
#2719=EDGE_CURVE('',#2219,#2221,#1389,.T.);
#2720=EDGE_CURVE('',#2221,#2222,#1390,.T.);
#2721=EDGE_CURVE('',#2220,#2222,#1391,.T.);
#2722=EDGE_CURVE('',#2223,#2219,#1392,.T.);
#2723=EDGE_CURVE('',#2223,#2224,#1393,.T.);
#2724=EDGE_CURVE('',#2224,#2221,#1394,.T.);
#2725=EDGE_CURVE('',#2225,#2223,#1395,.T.);
#2726=EDGE_CURVE('',#2225,#2226,#1396,.T.);
#2727=EDGE_CURVE('',#2226,#2224,#1397,.T.);
#2728=EDGE_CURVE('',#2227,#2225,#1398,.T.);
#2729=EDGE_CURVE('',#2227,#2228,#1399,.T.);
#2730=EDGE_CURVE('',#2228,#2226,#1400,.T.);
#2731=EDGE_CURVE('',#2229,#2227,#1401,.T.);
#2732=EDGE_CURVE('',#2229,#2230,#1402,.T.);
#2733=EDGE_CURVE('',#2230,#2228,#1403,.T.);
#2734=EDGE_CURVE('',#2220,#2229,#1404,.T.);
#2735=EDGE_CURVE('',#2222,#2230,#1405,.T.);
#2736=EDGE_CURVE('',#2231,#2231,#1887,.T.);
#2737=EDGE_CURVE('',#2232,#2232,#1888,.T.);
#2738=EDGE_CURVE('',#2232,#2231,#1406,.T.);
#2739=EDGE_CURVE('',#2233,#2233,#1889,.F.);
#2740=EDGE_CURVE('',#2233,#2232,#1407,.T.);
#2741=EDGE_CURVE('',#2234,#2234,#1890,.T.);
#2742=EDGE_CURVE('',#2234,#2233,#1408,.T.);
#2743=ORIENTED_EDGE('',*,*,#2235,.F.);
#2744=ORIENTED_EDGE('',*,*,#2236,.T.);
#2745=ORIENTED_EDGE('',*,*,#2237,.F.);
#2746=ORIENTED_EDGE('',*,*,#2236,.F.);
#2747=ORIENTED_EDGE('',*,*,#2238,.F.);
#2748=ORIENTED_EDGE('',*,*,#2239,.T.);
#2749=ORIENTED_EDGE('',*,*,#2240,.F.);
#2750=ORIENTED_EDGE('',*,*,#2239,.F.);
#2751=ORIENTED_EDGE('',*,*,#2241,.F.);
#2752=ORIENTED_EDGE('',*,*,#2242,.T.);
#2753=ORIENTED_EDGE('',*,*,#2243,.F.);
#2754=ORIENTED_EDGE('',*,*,#2242,.F.);
#2755=ORIENTED_EDGE('',*,*,#2244,.F.);
#2756=ORIENTED_EDGE('',*,*,#2245,.T.);
#2757=ORIENTED_EDGE('',*,*,#2246,.F.);
#2758=ORIENTED_EDGE('',*,*,#2245,.F.);
#2759=ORIENTED_EDGE('',*,*,#2247,.T.);
#2760=ORIENTED_EDGE('',*,*,#2248,.T.);
#2761=ORIENTED_EDGE('',*,*,#2249,.F.);
#2762=ORIENTED_EDGE('',*,*,#2250,.F.);
#2763=ORIENTED_EDGE('',*,*,#2251,.T.);
#2764=ORIENTED_EDGE('',*,*,#2250,.T.);
#2765=ORIENTED_EDGE('',*,*,#2252,.F.);
#2766=ORIENTED_EDGE('',*,*,#2253,.F.);
#2767=ORIENTED_EDGE('',*,*,#2254,.T.);
#2768=ORIENTED_EDGE('',*,*,#2253,.T.);
#2769=ORIENTED_EDGE('',*,*,#2255,.F.);
#2770=ORIENTED_EDGE('',*,*,#2256,.F.);
#2771=ORIENTED_EDGE('',*,*,#2257,.T.);
#2772=ORIENTED_EDGE('',*,*,#2256,.T.);
#2773=ORIENTED_EDGE('',*,*,#2258,.F.);
#2774=ORIENTED_EDGE('',*,*,#2248,.F.);
#2775=ORIENTED_EDGE('',*,*,#2258,.T.);
#2776=ORIENTED_EDGE('',*,*,#2255,.T.);
#2777=ORIENTED_EDGE('',*,*,#2252,.T.);
#2778=ORIENTED_EDGE('',*,*,#2249,.T.);
#2779=ORIENTED_EDGE('',*,*,#2237,.T.);
#2780=ORIENTED_EDGE('',*,*,#2240,.T.);
#2781=ORIENTED_EDGE('',*,*,#2243,.T.);
#2782=ORIENTED_EDGE('',*,*,#2246,.T.);
#2783=ORIENTED_EDGE('',*,*,#2257,.F.);
#2784=ORIENTED_EDGE('',*,*,#2247,.F.);
#2785=ORIENTED_EDGE('',*,*,#2251,.F.);
#2786=ORIENTED_EDGE('',*,*,#2254,.F.);
#2787=ORIENTED_EDGE('',*,*,#2235,.T.);
#2788=ORIENTED_EDGE('',*,*,#2238,.T.);
#2789=ORIENTED_EDGE('',*,*,#2241,.T.);
#2790=ORIENTED_EDGE('',*,*,#2244,.T.);
#2791=ORIENTED_EDGE('',*,*,#2259,.F.);
#2792=ORIENTED_EDGE('',*,*,#2260,.T.);
#2793=ORIENTED_EDGE('',*,*,#2261,.F.);
#2794=ORIENTED_EDGE('',*,*,#2260,.F.);
#2795=ORIENTED_EDGE('',*,*,#2259,.T.);
#2796=ORIENTED_EDGE('',*,*,#2262,.F.);
#2797=ORIENTED_EDGE('',*,*,#2263,.T.);
#2798=ORIENTED_EDGE('',*,*,#2264,.F.);
#2799=ORIENTED_EDGE('',*,*,#2263,.F.);
#2800=ORIENTED_EDGE('',*,*,#2262,.T.);
#2801=ORIENTED_EDGE('',*,*,#2265,.F.);
#2802=ORIENTED_EDGE('',*,*,#2266,.T.);
#2803=ORIENTED_EDGE('',*,*,#2267,.F.);
#2804=ORIENTED_EDGE('',*,*,#2266,.F.);
#2805=ORIENTED_EDGE('',*,*,#2265,.T.);
#2806=ORIENTED_EDGE('',*,*,#2268,.F.);
#2807=ORIENTED_EDGE('',*,*,#2269,.T.);
#2808=ORIENTED_EDGE('',*,*,#2270,.F.);
#2809=ORIENTED_EDGE('',*,*,#2269,.F.);
#2810=ORIENTED_EDGE('',*,*,#2268,.T.);
#2811=ORIENTED_EDGE('',*,*,#2271,.F.);
#2812=ORIENTED_EDGE('',*,*,#2272,.T.);
#2813=ORIENTED_EDGE('',*,*,#2273,.T.);
#2814=ORIENTED_EDGE('',*,*,#2272,.F.);
#2815=ORIENTED_EDGE('',*,*,#2273,.F.);
#2816=ORIENTED_EDGE('',*,*,#2274,.F.);
#2817=ORIENTED_EDGE('',*,*,#2275,.T.);
#2818=ORIENTED_EDGE('',*,*,#2276,.T.);
#2819=ORIENTED_EDGE('',*,*,#2275,.F.);
#2820=ORIENTED_EDGE('',*,*,#2276,.F.);
#2821=ORIENTED_EDGE('',*,*,#2277,.F.);
#2822=ORIENTED_EDGE('',*,*,#2278,.T.);
#2823=ORIENTED_EDGE('',*,*,#2279,.T.);
#2824=ORIENTED_EDGE('',*,*,#2278,.F.);
#2825=ORIENTED_EDGE('',*,*,#2279,.F.);
#2826=ORIENTED_EDGE('',*,*,#2280,.F.);
#2827=ORIENTED_EDGE('',*,*,#2281,.T.);
#2828=ORIENTED_EDGE('',*,*,#2282,.T.);
#2829=ORIENTED_EDGE('',*,*,#2281,.F.);
#2830=ORIENTED_EDGE('',*,*,#2282,.F.);
#2831=ORIENTED_EDGE('',*,*,#2283,.F.);
#2832=ORIENTED_EDGE('',*,*,#2284,.T.);
#2833=ORIENTED_EDGE('',*,*,#2285,.F.);
#2834=ORIENTED_EDGE('',*,*,#2284,.F.);
#2835=ORIENTED_EDGE('',*,*,#2286,.F.);
#2836=ORIENTED_EDGE('',*,*,#2287,.T.);
#2837=ORIENTED_EDGE('',*,*,#2288,.F.);
#2838=ORIENTED_EDGE('',*,*,#2287,.F.);
#2839=ORIENTED_EDGE('',*,*,#2289,.F.);
#2840=ORIENTED_EDGE('',*,*,#2290,.T.);
#2841=ORIENTED_EDGE('',*,*,#2291,.F.);
#2842=ORIENTED_EDGE('',*,*,#2290,.F.);
#2843=ORIENTED_EDGE('',*,*,#2292,.F.);
#2844=ORIENTED_EDGE('',*,*,#2293,.T.);
#2845=ORIENTED_EDGE('',*,*,#2294,.F.);
#2846=ORIENTED_EDGE('',*,*,#2293,.F.);
#2847=ORIENTED_EDGE('',*,*,#2295,.F.);
#2848=ORIENTED_EDGE('',*,*,#2296,.T.);
#2849=ORIENTED_EDGE('',*,*,#2297,.T.);
#2850=ORIENTED_EDGE('',*,*,#2298,.T.);
#2851=ORIENTED_EDGE('',*,*,#2299,.F.);
#2852=ORIENTED_EDGE('',*,*,#2300,.T.);
#2853=ORIENTED_EDGE('',*,*,#2301,.T.);
#2854=ORIENTED_EDGE('',*,*,#2302,.T.);
#2855=ORIENTED_EDGE('',*,*,#2303,.F.);
#2856=ORIENTED_EDGE('',*,*,#2304,.T.);
#2857=ORIENTED_EDGE('',*,*,#2305,.T.);
#2858=ORIENTED_EDGE('',*,*,#2306,.T.);
#2859=ORIENTED_EDGE('',*,*,#2307,.F.);
#2860=ORIENTED_EDGE('',*,*,#2308,.T.);
#2861=ORIENTED_EDGE('',*,*,#2309,.T.);
#2862=ORIENTED_EDGE('',*,*,#2310,.T.);
#2863=ORIENTED_EDGE('',*,*,#2311,.F.);
#2864=ORIENTED_EDGE('',*,*,#2306,.F.);
#2865=ORIENTED_EDGE('',*,*,#2312,.T.);
#2866=ORIENTED_EDGE('',*,*,#2296,.F.);
#2867=ORIENTED_EDGE('',*,*,#2294,.T.);
#2868=ORIENTED_EDGE('',*,*,#2313,.F.);
#2869=ORIENTED_EDGE('',*,*,#2302,.F.);
#2870=ORIENTED_EDGE('',*,*,#2314,.F.);
#2871=ORIENTED_EDGE('',*,*,#2308,.F.);
#2872=ORIENTED_EDGE('',*,*,#2288,.T.);
#2873=ORIENTED_EDGE('',*,*,#2309,.F.);
#2874=ORIENTED_EDGE('',*,*,#2314,.T.);
#2875=ORIENTED_EDGE('',*,*,#2301,.F.);
#2876=ORIENTED_EDGE('',*,*,#2315,.F.);
#2877=ORIENTED_EDGE('',*,*,#2298,.F.);
#2878=ORIENTED_EDGE('',*,*,#2316,.F.);
#2879=ORIENTED_EDGE('',*,*,#2304,.F.);
#2880=ORIENTED_EDGE('',*,*,#2310,.F.);
#2881=ORIENTED_EDGE('',*,*,#2315,.T.);
#2882=ORIENTED_EDGE('',*,*,#2300,.F.);
#2883=ORIENTED_EDGE('',*,*,#2286,.T.);
#2884=ORIENTED_EDGE('',*,*,#2292,.T.);
#2885=ORIENTED_EDGE('',*,*,#2305,.F.);
#2886=ORIENTED_EDGE('',*,*,#2316,.T.);
#2887=ORIENTED_EDGE('',*,*,#2297,.F.);
#2888=ORIENTED_EDGE('',*,*,#2312,.F.);
#2889=ORIENTED_EDGE('',*,*,#2317,.F.);
#2890=ORIENTED_EDGE('',*,*,#2318,.T.);
#2891=ORIENTED_EDGE('',*,*,#2319,.T.);
#2892=ORIENTED_EDGE('',*,*,#2320,.T.);
#2893=ORIENTED_EDGE('',*,*,#2321,.F.);
#2894=ORIENTED_EDGE('',*,*,#2322,.T.);
#2895=ORIENTED_EDGE('',*,*,#2323,.T.);
#2896=ORIENTED_EDGE('',*,*,#2324,.T.);
#2897=ORIENTED_EDGE('',*,*,#2325,.F.);
#2898=ORIENTED_EDGE('',*,*,#2326,.T.);
#2899=ORIENTED_EDGE('',*,*,#2327,.T.);
#2900=ORIENTED_EDGE('',*,*,#2328,.T.);
#2901=ORIENTED_EDGE('',*,*,#2329,.F.);
#2902=ORIENTED_EDGE('',*,*,#2330,.T.);
#2903=ORIENTED_EDGE('',*,*,#2331,.T.);
#2904=ORIENTED_EDGE('',*,*,#2332,.T.);
#2905=ORIENTED_EDGE('',*,*,#2333,.F.);
#2906=ORIENTED_EDGE('',*,*,#2328,.F.);
#2907=ORIENTED_EDGE('',*,*,#2334,.T.);
#2908=ORIENTED_EDGE('',*,*,#2318,.F.);
#2909=ORIENTED_EDGE('',*,*,#2285,.T.);
#2910=ORIENTED_EDGE('',*,*,#2335,.F.);
#2911=ORIENTED_EDGE('',*,*,#2324,.F.);
#2912=ORIENTED_EDGE('',*,*,#2336,.F.);
#2913=ORIENTED_EDGE('',*,*,#2330,.F.);
#2914=ORIENTED_EDGE('',*,*,#2291,.T.);
#2915=ORIENTED_EDGE('',*,*,#2331,.F.);
#2916=ORIENTED_EDGE('',*,*,#2336,.T.);
#2917=ORIENTED_EDGE('',*,*,#2323,.F.);
#2918=ORIENTED_EDGE('',*,*,#2337,.F.);
#2919=ORIENTED_EDGE('',*,*,#2320,.F.);
#2920=ORIENTED_EDGE('',*,*,#2338,.F.);
#2921=ORIENTED_EDGE('',*,*,#2326,.F.);
#2922=ORIENTED_EDGE('',*,*,#2332,.F.);
#2923=ORIENTED_EDGE('',*,*,#2337,.T.);
#2924=ORIENTED_EDGE('',*,*,#2322,.F.);
#2925=ORIENTED_EDGE('',*,*,#2283,.T.);
#2926=ORIENTED_EDGE('',*,*,#2289,.T.);
#2927=ORIENTED_EDGE('',*,*,#2327,.F.);
#2928=ORIENTED_EDGE('',*,*,#2338,.T.);
#2929=ORIENTED_EDGE('',*,*,#2319,.F.);
#2930=ORIENTED_EDGE('',*,*,#2334,.F.);
#2931=ORIENTED_EDGE('',*,*,#2339,.F.);
#2932=ORIENTED_EDGE('',*,*,#2340,.T.);
#2933=ORIENTED_EDGE('',*,*,#2341,.T.);
#2934=ORIENTED_EDGE('',*,*,#2340,.F.);
#2935=ORIENTED_EDGE('',*,*,#2342,.F.);
#2936=ORIENTED_EDGE('',*,*,#2343,.T.);
#2937=ORIENTED_EDGE('',*,*,#2344,.T.);
#2938=ORIENTED_EDGE('',*,*,#2343,.F.);
#2939=ORIENTED_EDGE('',*,*,#2311,.T.);
#2940=ORIENTED_EDGE('',*,*,#2295,.T.);
#2941=ORIENTED_EDGE('',*,*,#2299,.T.);
#2942=ORIENTED_EDGE('',*,*,#2313,.T.);
#2943=ORIENTED_EDGE('',*,*,#2307,.T.);
#2944=ORIENTED_EDGE('',*,*,#2303,.T.);
#2945=ORIENTED_EDGE('',*,*,#2333,.T.);
#2946=ORIENTED_EDGE('',*,*,#2317,.T.);
#2947=ORIENTED_EDGE('',*,*,#2321,.T.);
#2948=ORIENTED_EDGE('',*,*,#2335,.T.);
#2949=ORIENTED_EDGE('',*,*,#2329,.T.);
#2950=ORIENTED_EDGE('',*,*,#2325,.T.);
#2951=ORIENTED_EDGE('',*,*,#2342,.T.);
#2952=ORIENTED_EDGE('',*,*,#2339,.T.);
#2953=ORIENTED_EDGE('',*,*,#2270,.T.);
#2954=ORIENTED_EDGE('',*,*,#2267,.T.);
#2955=ORIENTED_EDGE('',*,*,#2264,.T.);
#2956=ORIENTED_EDGE('',*,*,#2261,.T.);
#2957=ORIENTED_EDGE('',*,*,#2344,.F.);
#2958=ORIENTED_EDGE('',*,*,#2341,.F.);
#2959=ORIENTED_EDGE('',*,*,#2280,.T.);
#2960=ORIENTED_EDGE('',*,*,#2277,.T.);
#2961=ORIENTED_EDGE('',*,*,#2274,.T.);
#2962=ORIENTED_EDGE('',*,*,#2271,.T.);
#2963=ORIENTED_EDGE('',*,*,#2345,.F.);
#2964=ORIENTED_EDGE('',*,*,#2346,.T.);
#2965=ORIENTED_EDGE('',*,*,#2347,.T.);
#2966=ORIENTED_EDGE('',*,*,#2346,.F.);
#2967=ORIENTED_EDGE('',*,*,#2348,.F.);
#2968=ORIENTED_EDGE('',*,*,#2349,.T.);
#2969=ORIENTED_EDGE('',*,*,#2350,.T.);
#2970=ORIENTED_EDGE('',*,*,#2349,.F.);
#2971=ORIENTED_EDGE('',*,*,#2348,.T.);
#2972=ORIENTED_EDGE('',*,*,#2345,.T.);
#2973=ORIENTED_EDGE('',*,*,#2350,.F.);
#2974=ORIENTED_EDGE('',*,*,#2347,.F.);
#2975=ORIENTED_EDGE('',*,*,#2351,.F.);
#2976=ORIENTED_EDGE('',*,*,#2352,.T.);
#2977=ORIENTED_EDGE('',*,*,#2353,.F.);
#2978=ORIENTED_EDGE('',*,*,#2352,.F.);
#2979=ORIENTED_EDGE('',*,*,#2354,.F.);
#2980=ORIENTED_EDGE('',*,*,#2355,.T.);
#2981=ORIENTED_EDGE('',*,*,#2356,.F.);
#2982=ORIENTED_EDGE('',*,*,#2355,.F.);
#2983=ORIENTED_EDGE('',*,*,#2357,.F.);
#2984=ORIENTED_EDGE('',*,*,#2358,.T.);
#2985=ORIENTED_EDGE('',*,*,#2359,.F.);
#2986=ORIENTED_EDGE('',*,*,#2358,.F.);
#2987=ORIENTED_EDGE('',*,*,#2360,.F.);
#2988=ORIENTED_EDGE('',*,*,#2361,.T.);
#2989=ORIENTED_EDGE('',*,*,#2362,.F.);
#2990=ORIENTED_EDGE('',*,*,#2361,.F.);
#2991=ORIENTED_EDGE('',*,*,#2363,.F.);
#2992=ORIENTED_EDGE('',*,*,#2364,.T.);
#2993=ORIENTED_EDGE('',*,*,#2365,.F.);
#2994=ORIENTED_EDGE('',*,*,#2364,.F.);
#2995=ORIENTED_EDGE('',*,*,#2363,.T.);
#2996=ORIENTED_EDGE('',*,*,#2366,.T.);
#2997=ORIENTED_EDGE('',*,*,#2367,.F.);
#2998=ORIENTED_EDGE('',*,*,#2368,.T.);
#2999=ORIENTED_EDGE('',*,*,#2369,.T.);
#3000=ORIENTED_EDGE('',*,*,#2368,.F.);
#3001=ORIENTED_EDGE('',*,*,#2369,.F.);
#3002=ORIENTED_EDGE('',*,*,#2370,.F.);
#3003=ORIENTED_EDGE('',*,*,#2366,.F.);
#3004=ORIENTED_EDGE('',*,*,#2371,.T.);
#3005=ORIENTED_EDGE('',*,*,#2370,.T.);
#3006=ORIENTED_EDGE('',*,*,#2371,.F.);
#3007=ORIENTED_EDGE('',*,*,#2372,.F.);
#3008=ORIENTED_EDGE('',*,*,#2373,.T.);
#3009=ORIENTED_EDGE('',*,*,#2374,.T.);
#3010=ORIENTED_EDGE('',*,*,#2373,.F.);
#3011=ORIENTED_EDGE('',*,*,#2372,.T.);
#3012=ORIENTED_EDGE('',*,*,#2365,.T.);
#3013=ORIENTED_EDGE('',*,*,#2362,.T.);
#3014=ORIENTED_EDGE('',*,*,#2359,.T.);
#3015=ORIENTED_EDGE('',*,*,#2356,.T.);
#3016=ORIENTED_EDGE('',*,*,#2353,.T.);
#3017=ORIENTED_EDGE('',*,*,#2374,.F.);
#3018=ORIENTED_EDGE('',*,*,#2367,.T.);
#3019=ORIENTED_EDGE('',*,*,#2360,.T.);
#3020=ORIENTED_EDGE('',*,*,#2357,.T.);
#3021=ORIENTED_EDGE('',*,*,#2354,.T.);
#3022=ORIENTED_EDGE('',*,*,#2351,.T.);
#3023=ORIENTED_EDGE('',*,*,#2375,.F.);
#3024=ORIENTED_EDGE('',*,*,#2376,.T.);
#3025=ORIENTED_EDGE('',*,*,#2377,.T.);
#3026=ORIENTED_EDGE('',*,*,#2376,.F.);
#3027=ORIENTED_EDGE('',*,*,#2378,.F.);
#3028=ORIENTED_EDGE('',*,*,#2379,.T.);
#3029=ORIENTED_EDGE('',*,*,#2380,.T.);
#3030=ORIENTED_EDGE('',*,*,#2379,.F.);
#3031=ORIENTED_EDGE('',*,*,#2378,.T.);
#3032=ORIENTED_EDGE('',*,*,#2375,.T.);
#3033=ORIENTED_EDGE('',*,*,#2380,.F.);
#3034=ORIENTED_EDGE('',*,*,#2377,.F.);
#3035=ORIENTED_EDGE('',*,*,#2381,.F.);
#3036=ORIENTED_EDGE('',*,*,#2382,.T.);
#3037=ORIENTED_EDGE('',*,*,#2383,.F.);
#3038=ORIENTED_EDGE('',*,*,#2382,.F.);
#3039=ORIENTED_EDGE('',*,*,#2381,.T.);
#3040=ORIENTED_EDGE('',*,*,#2384,.F.);
#3041=ORIENTED_EDGE('',*,*,#2385,.F.);
#3042=ORIENTED_EDGE('',*,*,#2386,.T.);
#3043=ORIENTED_EDGE('',*,*,#2387,.F.);
#3044=ORIENTED_EDGE('',*,*,#2386,.F.);
#3045=ORIENTED_EDGE('',*,*,#2385,.T.);
#3046=ORIENTED_EDGE('',*,*,#2388,.F.);
#3047=ORIENTED_EDGE('',*,*,#2389,.F.);
#3048=ORIENTED_EDGE('',*,*,#2390,.T.);
#3049=ORIENTED_EDGE('',*,*,#2391,.F.);
#3050=ORIENTED_EDGE('',*,*,#2390,.F.);
#3051=ORIENTED_EDGE('',*,*,#2389,.T.);
#3052=ORIENTED_EDGE('',*,*,#2392,.F.);
#3053=ORIENTED_EDGE('',*,*,#2393,.F.);
#3054=ORIENTED_EDGE('',*,*,#2394,.T.);
#3055=ORIENTED_EDGE('',*,*,#2395,.F.);
#3056=ORIENTED_EDGE('',*,*,#2394,.F.);
#3057=ORIENTED_EDGE('',*,*,#2393,.T.);
#3058=ORIENTED_EDGE('',*,*,#2396,.F.);
#3059=ORIENTED_EDGE('',*,*,#2397,.F.);
#3060=ORIENTED_EDGE('',*,*,#2398,.T.);
#3061=ORIENTED_EDGE('',*,*,#2384,.T.);
#3062=ORIENTED_EDGE('',*,*,#2398,.F.);
#3063=ORIENTED_EDGE('',*,*,#2399,.F.);
#3064=ORIENTED_EDGE('',*,*,#2400,.T.);
#3065=ORIENTED_EDGE('',*,*,#2388,.T.);
#3066=ORIENTED_EDGE('',*,*,#2400,.F.);
#3067=ORIENTED_EDGE('',*,*,#2401,.F.);
#3068=ORIENTED_EDGE('',*,*,#2402,.T.);
#3069=ORIENTED_EDGE('',*,*,#2392,.T.);
#3070=ORIENTED_EDGE('',*,*,#2402,.F.);
#3071=ORIENTED_EDGE('',*,*,#2403,.F.);
#3072=ORIENTED_EDGE('',*,*,#2404,.T.);
#3073=ORIENTED_EDGE('',*,*,#2396,.T.);
#3074=ORIENTED_EDGE('',*,*,#2404,.F.);
#3075=ORIENTED_EDGE('',*,*,#2405,.T.);
#3076=ORIENTED_EDGE('',*,*,#2406,.T.);
#3077=ORIENTED_EDGE('',*,*,#2406,.F.);
#3078=ORIENTED_EDGE('',*,*,#2407,.T.);
#3079=ORIENTED_EDGE('',*,*,#2408,.T.);
#3080=ORIENTED_EDGE('',*,*,#2407,.F.);
#3081=ORIENTED_EDGE('',*,*,#2409,.F.);
#3082=ORIENTED_EDGE('',*,*,#2410,.T.);
#3083=ORIENTED_EDGE('',*,*,#2411,.T.);
#3084=ORIENTED_EDGE('',*,*,#2410,.F.);
#3085=ORIENTED_EDGE('',*,*,#2411,.F.);
#3086=ORIENTED_EDGE('',*,*,#2408,.F.);
#3087=ORIENTED_EDGE('',*,*,#2405,.F.);
#3088=ORIENTED_EDGE('',*,*,#2412,.T.);
#3089=ORIENTED_EDGE('',*,*,#2413,.T.);
#3090=ORIENTED_EDGE('',*,*,#2412,.F.);
#3091=ORIENTED_EDGE('',*,*,#2413,.F.);
#3092=ORIENTED_EDGE('',*,*,#2414,.F.);
#3093=ORIENTED_EDGE('',*,*,#2415,.T.);
#3094=ORIENTED_EDGE('',*,*,#2416,.T.);
#3095=ORIENTED_EDGE('',*,*,#2415,.F.);
#3096=ORIENTED_EDGE('',*,*,#2414,.T.);
#3097=ORIENTED_EDGE('',*,*,#2395,.T.);
#3098=ORIENTED_EDGE('',*,*,#2391,.T.);
#3099=ORIENTED_EDGE('',*,*,#2387,.T.);
#3100=ORIENTED_EDGE('',*,*,#2383,.T.);
#3101=ORIENTED_EDGE('',*,*,#2416,.F.);
#3102=ORIENTED_EDGE('',*,*,#2409,.T.);
#3103=ORIENTED_EDGE('',*,*,#2403,.T.);
#3104=ORIENTED_EDGE('',*,*,#2401,.T.);
#3105=ORIENTED_EDGE('',*,*,#2399,.T.);
#3106=ORIENTED_EDGE('',*,*,#2397,.T.);
#3107=ORIENTED_EDGE('',*,*,#2417,.T.);
#3108=ORIENTED_EDGE('',*,*,#2418,.T.);
#3109=ORIENTED_EDGE('',*,*,#2419,.F.);
#3110=ORIENTED_EDGE('',*,*,#2420,.F.);
#3111=ORIENTED_EDGE('',*,*,#2421,.T.);
#3112=ORIENTED_EDGE('',*,*,#2420,.T.);
#3113=ORIENTED_EDGE('',*,*,#2422,.F.);
#3114=ORIENTED_EDGE('',*,*,#2423,.F.);
#3115=ORIENTED_EDGE('',*,*,#2424,.T.);
#3116=ORIENTED_EDGE('',*,*,#2423,.T.);
#3117=ORIENTED_EDGE('',*,*,#2425,.F.);
#3118=ORIENTED_EDGE('',*,*,#2426,.F.);
#3119=ORIENTED_EDGE('',*,*,#2427,.T.);
#3120=ORIENTED_EDGE('',*,*,#2426,.T.);
#3121=ORIENTED_EDGE('',*,*,#2428,.F.);
#3122=ORIENTED_EDGE('',*,*,#2418,.F.);
#3123=ORIENTED_EDGE('',*,*,#2428,.T.);
#3124=ORIENTED_EDGE('',*,*,#2425,.T.);
#3125=ORIENTED_EDGE('',*,*,#2422,.T.);
#3126=ORIENTED_EDGE('',*,*,#2419,.T.);
#3127=ORIENTED_EDGE('',*,*,#2427,.F.);
#3128=ORIENTED_EDGE('',*,*,#2417,.F.);
#3129=ORIENTED_EDGE('',*,*,#2421,.F.);
#3130=ORIENTED_EDGE('',*,*,#2424,.F.);
#3131=ORIENTED_EDGE('',*,*,#2429,.T.);
#3132=ORIENTED_EDGE('',*,*,#2430,.T.);
#3133=ORIENTED_EDGE('',*,*,#2431,.F.);
#3134=ORIENTED_EDGE('',*,*,#2432,.F.);
#3135=ORIENTED_EDGE('',*,*,#2433,.T.);
#3136=ORIENTED_EDGE('',*,*,#2432,.T.);
#3137=ORIENTED_EDGE('',*,*,#2434,.F.);
#3138=ORIENTED_EDGE('',*,*,#2435,.F.);
#3139=ORIENTED_EDGE('',*,*,#2436,.T.);
#3140=ORIENTED_EDGE('',*,*,#2435,.T.);
#3141=ORIENTED_EDGE('',*,*,#2437,.F.);
#3142=ORIENTED_EDGE('',*,*,#2438,.F.);
#3143=ORIENTED_EDGE('',*,*,#2439,.T.);
#3144=ORIENTED_EDGE('',*,*,#2438,.T.);
#3145=ORIENTED_EDGE('',*,*,#2440,.F.);
#3146=ORIENTED_EDGE('',*,*,#2430,.F.);
#3147=ORIENTED_EDGE('',*,*,#2440,.T.);
#3148=ORIENTED_EDGE('',*,*,#2437,.T.);
#3149=ORIENTED_EDGE('',*,*,#2434,.T.);
#3150=ORIENTED_EDGE('',*,*,#2431,.T.);
#3151=ORIENTED_EDGE('',*,*,#2439,.F.);
#3152=ORIENTED_EDGE('',*,*,#2429,.F.);
#3153=ORIENTED_EDGE('',*,*,#2433,.F.);
#3154=ORIENTED_EDGE('',*,*,#2436,.F.);
#3155=ORIENTED_EDGE('',*,*,#2441,.F.);
#3156=ORIENTED_EDGE('',*,*,#2442,.F.);
#3157=ORIENTED_EDGE('',*,*,#2443,.T.);
#3158=ORIENTED_EDGE('',*,*,#2444,.F.);
#3159=ORIENTED_EDGE('',*,*,#2445,.F.);
#3160=ORIENTED_EDGE('',*,*,#2443,.F.);
#3161=ORIENTED_EDGE('',*,*,#2444,.T.);
#3162=ORIENTED_EDGE('',*,*,#2445,.T.);
#3163=ORIENTED_EDGE('',*,*,#2446,.T.);
#3164=ORIENTED_EDGE('',*,*,#2447,.T.);
#3165=ORIENTED_EDGE('',*,*,#2446,.F.);
#3166=ORIENTED_EDGE('',*,*,#2448,.T.);
#3167=ORIENTED_EDGE('',*,*,#2449,.T.);
#3168=ORIENTED_EDGE('',*,*,#2450,.F.);
#3169=ORIENTED_EDGE('',*,*,#2449,.F.);
#3170=ORIENTED_EDGE('',*,*,#2450,.T.);
#3171=ORIENTED_EDGE('',*,*,#2451,.T.);
#3172=ORIENTED_EDGE('',*,*,#2452,.F.);
#3173=ORIENTED_EDGE('',*,*,#2451,.F.);
#3174=ORIENTED_EDGE('',*,*,#2447,.F.);
#3175=ORIENTED_EDGE('',*,*,#2452,.T.);
#3176=ORIENTED_EDGE('',*,*,#2453,.F.);
#3177=ORIENTED_EDGE('',*,*,#2454,.T.);
#3178=ORIENTED_EDGE('',*,*,#2441,.T.);
#3179=ORIENTED_EDGE('',*,*,#2442,.T.);
#3180=ORIENTED_EDGE('',*,*,#2454,.F.);
#3181=ORIENTED_EDGE('',*,*,#2453,.T.);
#3182=ORIENTED_EDGE('',*,*,#2455,.F.);
#3183=ORIENTED_EDGE('',*,*,#2455,.T.);
#3184=ORIENTED_EDGE('',*,*,#2456,.T.);
#3185=ORIENTED_EDGE('',*,*,#2448,.F.);
#3186=ORIENTED_EDGE('',*,*,#2456,.F.);
#3187=ORIENTED_EDGE('',*,*,#2457,.F.);
#3188=ORIENTED_EDGE('',*,*,#2458,.F.);
#3189=ORIENTED_EDGE('',*,*,#2459,.T.);
#3190=ORIENTED_EDGE('',*,*,#2460,.F.);
#3191=ORIENTED_EDGE('',*,*,#2461,.F.);
#3192=ORIENTED_EDGE('',*,*,#2459,.F.);
#3193=ORIENTED_EDGE('',*,*,#2462,.T.);
#3194=ORIENTED_EDGE('',*,*,#2463,.T.);
#3195=ORIENTED_EDGE('',*,*,#2460,.T.);
#3196=ORIENTED_EDGE('',*,*,#2461,.T.);
#3197=ORIENTED_EDGE('',*,*,#2463,.F.);
#3198=ORIENTED_EDGE('',*,*,#2464,.F.);
#3199=ORIENTED_EDGE('',*,*,#2465,.T.);
#3200=ORIENTED_EDGE('',*,*,#2466,.F.);
#3201=ORIENTED_EDGE('',*,*,#2467,.T.);
#3202=ORIENTED_EDGE('',*,*,#2464,.T.);
#3203=ORIENTED_EDGE('',*,*,#2467,.F.);
#3204=ORIENTED_EDGE('',*,*,#2468,.F.);
#3205=ORIENTED_EDGE('',*,*,#2469,.T.);
#3206=ORIENTED_EDGE('',*,*,#2466,.T.);
#3207=ORIENTED_EDGE('',*,*,#2469,.F.);
#3208=ORIENTED_EDGE('',*,*,#2470,.F.);
#3209=ORIENTED_EDGE('',*,*,#2471,.T.);
#3210=ORIENTED_EDGE('',*,*,#2468,.T.);
#3211=ORIENTED_EDGE('',*,*,#2471,.F.);
#3212=ORIENTED_EDGE('',*,*,#2470,.T.);
#3213=ORIENTED_EDGE('',*,*,#2462,.F.);
#3214=ORIENTED_EDGE('',*,*,#2457,.T.);
#3215=ORIENTED_EDGE('',*,*,#2458,.T.);
#3216=ORIENTED_EDGE('',*,*,#2472,.T.);
#3217=ORIENTED_EDGE('',*,*,#2465,.F.);
#3218=ORIENTED_EDGE('',*,*,#2472,.F.);
#3219=ORIENTED_EDGE('',*,*,#2473,.T.);
#3220=ORIENTED_EDGE('',*,*,#2473,.F.);
#3221=ORIENTED_EDGE('',*,*,#2474,.T.);
#3222=ORIENTED_EDGE('',*,*,#2474,.F.);
#3223=ORIENTED_EDGE('',*,*,#2475,.T.);
#3224=ORIENTED_EDGE('',*,*,#2475,.F.);
#3225=ORIENTED_EDGE('',*,*,#2476,.T.);
#3226=ORIENTED_EDGE('',*,*,#2476,.F.);
#3227=ORIENTED_EDGE('',*,*,#2477,.T.);
#3228=ORIENTED_EDGE('',*,*,#2477,.F.);
#3229=ORIENTED_EDGE('',*,*,#2478,.T.);
#3230=ORIENTED_EDGE('',*,*,#2478,.F.);
#3231=ORIENTED_EDGE('',*,*,#2479,.T.);
#3232=ORIENTED_EDGE('',*,*,#2479,.F.);
#3233=ORIENTED_EDGE('',*,*,#2480,.T.);
#3234=ORIENTED_EDGE('',*,*,#2480,.F.);
#3235=ORIENTED_EDGE('',*,*,#2481,.F.);
#3236=ORIENTED_EDGE('',*,*,#2482,.F.);
#3237=ORIENTED_EDGE('',*,*,#2483,.F.);
#3238=ORIENTED_EDGE('',*,*,#2484,.F.);
#3239=ORIENTED_EDGE('',*,*,#2483,.T.);
#3240=ORIENTED_EDGE('',*,*,#2485,.F.);
#3241=ORIENTED_EDGE('',*,*,#2486,.T.);
#3242=ORIENTED_EDGE('',*,*,#2487,.F.);
#3243=ORIENTED_EDGE('',*,*,#2488,.T.);
#3244=ORIENTED_EDGE('',*,*,#2489,.F.);
#3245=ORIENTED_EDGE('',*,*,#2490,.T.);
#3246=ORIENTED_EDGE('',*,*,#2491,.T.);
#3247=ORIENTED_EDGE('',*,*,#2492,.F.);
#3248=ORIENTED_EDGE('',*,*,#2491,.F.);
#3249=ORIENTED_EDGE('',*,*,#2493,.T.);
#3250=ORIENTED_EDGE('',*,*,#2494,.F.);
#3251=ORIENTED_EDGE('',*,*,#2495,.T.);
#3252=ORIENTED_EDGE('',*,*,#2496,.F.);
#3253=ORIENTED_EDGE('',*,*,#2497,.T.);
#3254=ORIENTED_EDGE('',*,*,#2498,.F.);
#3255=ORIENTED_EDGE('',*,*,#2499,.T.);
#3256=ORIENTED_EDGE('',*,*,#2500,.F.);
#3257=ORIENTED_EDGE('',*,*,#2501,.T.);
#3258=ORIENTED_EDGE('',*,*,#2502,.F.);
#3259=ORIENTED_EDGE('',*,*,#2482,.T.);
#3260=ORIENTED_EDGE('',*,*,#2503,.T.);
#3261=ORIENTED_EDGE('',*,*,#2504,.T.);
#3262=ORIENTED_EDGE('',*,*,#2485,.T.);
#3263=ORIENTED_EDGE('',*,*,#2505,.F.);
#3264=ORIENTED_EDGE('',*,*,#2506,.F.);
#3265=ORIENTED_EDGE('',*,*,#2486,.F.);
#3266=ORIENTED_EDGE('',*,*,#2504,.F.);
#3267=ORIENTED_EDGE('',*,*,#2506,.T.);
#3268=ORIENTED_EDGE('',*,*,#2507,.T.);
#3269=ORIENTED_EDGE('',*,*,#2508,.T.);
#3270=ORIENTED_EDGE('',*,*,#2487,.T.);
#3271=ORIENTED_EDGE('',*,*,#2509,.F.);
#3272=ORIENTED_EDGE('',*,*,#2510,.F.);
#3273=ORIENTED_EDGE('',*,*,#2488,.F.);
#3274=ORIENTED_EDGE('',*,*,#2508,.F.);
#3275=ORIENTED_EDGE('',*,*,#2510,.T.);
#3276=ORIENTED_EDGE('',*,*,#2511,.T.);
#3277=ORIENTED_EDGE('',*,*,#2512,.T.);
#3278=ORIENTED_EDGE('',*,*,#2489,.T.);
#3279=ORIENTED_EDGE('',*,*,#2513,.F.);
#3280=ORIENTED_EDGE('',*,*,#2514,.F.);
#3281=ORIENTED_EDGE('',*,*,#2493,.F.);
#3282=ORIENTED_EDGE('',*,*,#2490,.F.);
#3283=ORIENTED_EDGE('',*,*,#2512,.F.);
#3284=ORIENTED_EDGE('',*,*,#2515,.F.);
#3285=ORIENTED_EDGE('',*,*,#2514,.T.);
#3286=ORIENTED_EDGE('',*,*,#2516,.T.);
#3287=ORIENTED_EDGE('',*,*,#2517,.T.);
#3288=ORIENTED_EDGE('',*,*,#2494,.T.);
#3289=ORIENTED_EDGE('',*,*,#2518,.F.);
#3290=ORIENTED_EDGE('',*,*,#2519,.F.);
#3291=ORIENTED_EDGE('',*,*,#2495,.F.);
#3292=ORIENTED_EDGE('',*,*,#2517,.F.);
#3293=ORIENTED_EDGE('',*,*,#2519,.T.);
#3294=ORIENTED_EDGE('',*,*,#2520,.T.);
#3295=ORIENTED_EDGE('',*,*,#2521,.T.);
#3296=ORIENTED_EDGE('',*,*,#2496,.T.);
#3297=ORIENTED_EDGE('',*,*,#2522,.F.);
#3298=ORIENTED_EDGE('',*,*,#2523,.F.);
#3299=ORIENTED_EDGE('',*,*,#2497,.F.);
#3300=ORIENTED_EDGE('',*,*,#2521,.F.);
#3301=ORIENTED_EDGE('',*,*,#2523,.T.);
#3302=ORIENTED_EDGE('',*,*,#2524,.T.);
#3303=ORIENTED_EDGE('',*,*,#2525,.T.);
#3304=ORIENTED_EDGE('',*,*,#2498,.T.);
#3305=ORIENTED_EDGE('',*,*,#2499,.F.);
#3306=ORIENTED_EDGE('',*,*,#2525,.F.);
#3307=ORIENTED_EDGE('',*,*,#2526,.F.);
#3308=ORIENTED_EDGE('',*,*,#2527,.F.);
#3309=ORIENTED_EDGE('',*,*,#2528,.F.);
#3310=ORIENTED_EDGE('',*,*,#2529,.T.);
#3311=ORIENTED_EDGE('',*,*,#2515,.T.);
#3312=ORIENTED_EDGE('',*,*,#2511,.F.);
#3313=ORIENTED_EDGE('',*,*,#2509,.T.);
#3314=ORIENTED_EDGE('',*,*,#2507,.F.);
#3315=ORIENTED_EDGE('',*,*,#2505,.T.);
#3316=ORIENTED_EDGE('',*,*,#2503,.F.);
#3317=ORIENTED_EDGE('',*,*,#2481,.T.);
#3318=ORIENTED_EDGE('',*,*,#2530,.F.);
#3319=ORIENTED_EDGE('',*,*,#2531,.T.);
#3320=ORIENTED_EDGE('',*,*,#2532,.F.);
#3321=ORIENTED_EDGE('',*,*,#2526,.T.);
#3322=ORIENTED_EDGE('',*,*,#2524,.F.);
#3323=ORIENTED_EDGE('',*,*,#2522,.T.);
#3324=ORIENTED_EDGE('',*,*,#2520,.F.);
#3325=ORIENTED_EDGE('',*,*,#2518,.T.);
#3326=ORIENTED_EDGE('',*,*,#2516,.F.);
#3327=ORIENTED_EDGE('',*,*,#2513,.T.);
#3328=ORIENTED_EDGE('',*,*,#2529,.F.);
#3329=ORIENTED_EDGE('',*,*,#2484,.T.);
#3330=ORIENTED_EDGE('',*,*,#2502,.T.);
#3331=ORIENTED_EDGE('',*,*,#2533,.T.);
#3332=ORIENTED_EDGE('',*,*,#2530,.T.);
#3333=ORIENTED_EDGE('',*,*,#2501,.F.);
#3334=ORIENTED_EDGE('',*,*,#2534,.F.);
#3335=ORIENTED_EDGE('',*,*,#2531,.F.);
#3336=ORIENTED_EDGE('',*,*,#2533,.F.);
#3337=ORIENTED_EDGE('',*,*,#2492,.T.);
#3338=ORIENTED_EDGE('',*,*,#2528,.T.);
#3339=ORIENTED_EDGE('',*,*,#2527,.T.);
#3340=ORIENTED_EDGE('',*,*,#2532,.T.);
#3341=ORIENTED_EDGE('',*,*,#2534,.T.);
#3342=ORIENTED_EDGE('',*,*,#2500,.T.);
#3343=ORIENTED_EDGE('',*,*,#2535,.F.);
#3344=ORIENTED_EDGE('',*,*,#2536,.T.);
#3345=ORIENTED_EDGE('',*,*,#2537,.F.);
#3346=ORIENTED_EDGE('',*,*,#2538,.T.);
#3347=ORIENTED_EDGE('',*,*,#2535,.T.);
#3348=ORIENTED_EDGE('',*,*,#2538,.F.);
#3349=ORIENTED_EDGE('',*,*,#2537,.T.);
#3350=ORIENTED_EDGE('',*,*,#2539,.F.);
#3351=ORIENTED_EDGE('',*,*,#2539,.T.);
#3352=ORIENTED_EDGE('',*,*,#2540,.T.);
#3353=ORIENTED_EDGE('',*,*,#2536,.F.);
#3354=ORIENTED_EDGE('',*,*,#2540,.F.);
#3355=ORIENTED_EDGE('',*,*,#2541,.F.);
#3356=ORIENTED_EDGE('',*,*,#2542,.T.);
#3357=ORIENTED_EDGE('',*,*,#2543,.F.);
#3358=ORIENTED_EDGE('',*,*,#2544,.T.);
#3359=ORIENTED_EDGE('',*,*,#2541,.T.);
#3360=ORIENTED_EDGE('',*,*,#2544,.F.);
#3361=ORIENTED_EDGE('',*,*,#2543,.T.);
#3362=ORIENTED_EDGE('',*,*,#2545,.F.);
#3363=ORIENTED_EDGE('',*,*,#2545,.T.);
#3364=ORIENTED_EDGE('',*,*,#2546,.T.);
#3365=ORIENTED_EDGE('',*,*,#2542,.F.);
#3366=ORIENTED_EDGE('',*,*,#2546,.F.);
#3367=ORIENTED_EDGE('',*,*,#2547,.F.);
#3368=ORIENTED_EDGE('',*,*,#2548,.F.);
#3369=ORIENTED_EDGE('',*,*,#2549,.T.);
#3370=ORIENTED_EDGE('',*,*,#2547,.T.);
#3371=ORIENTED_EDGE('',*,*,#2549,.F.);
#3372=ORIENTED_EDGE('',*,*,#2550,.F.);
#3373=ORIENTED_EDGE('',*,*,#2551,.T.);
#3374=ORIENTED_EDGE('',*,*,#2548,.T.);
#3375=ORIENTED_EDGE('',*,*,#2551,.F.);
#3376=ORIENTED_EDGE('',*,*,#2552,.F.);
#3377=ORIENTED_EDGE('',*,*,#2553,.T.);
#3378=ORIENTED_EDGE('',*,*,#2550,.T.);
#3379=ORIENTED_EDGE('',*,*,#2553,.F.);
#3380=ORIENTED_EDGE('',*,*,#2552,.T.);
#3381=ORIENTED_EDGE('',*,*,#2554,.F.);
#3382=ORIENTED_EDGE('',*,*,#2555,.F.);
#3383=ORIENTED_EDGE('',*,*,#2556,.T.);
#3384=ORIENTED_EDGE('',*,*,#2554,.T.);
#3385=ORIENTED_EDGE('',*,*,#2556,.F.);
#3386=ORIENTED_EDGE('',*,*,#2557,.F.);
#3387=ORIENTED_EDGE('',*,*,#2558,.T.);
#3388=ORIENTED_EDGE('',*,*,#2555,.T.);
#3389=ORIENTED_EDGE('',*,*,#2558,.F.);
#3390=ORIENTED_EDGE('',*,*,#2559,.F.);
#3391=ORIENTED_EDGE('',*,*,#2560,.T.);
#3392=ORIENTED_EDGE('',*,*,#2557,.T.);
#3393=ORIENTED_EDGE('',*,*,#2560,.F.);
#3394=ORIENTED_EDGE('',*,*,#2559,.T.);
#3395=ORIENTED_EDGE('',*,*,#2561,.T.);
#3396=ORIENTED_EDGE('',*,*,#2562,.T.);
#3397=ORIENTED_EDGE('',*,*,#2563,.T.);
#3398=ORIENTED_EDGE('',*,*,#2564,.F.);
#3399=ORIENTED_EDGE('',*,*,#2565,.T.);
#3400=ORIENTED_EDGE('',*,*,#2566,.T.);
#3401=ORIENTED_EDGE('',*,*,#2567,.T.);
#3402=ORIENTED_EDGE('',*,*,#2562,.F.);
#3403=ORIENTED_EDGE('',*,*,#2568,.T.);
#3404=ORIENTED_EDGE('',*,*,#2569,.T.);
#3405=ORIENTED_EDGE('',*,*,#2570,.T.);
#3406=ORIENTED_EDGE('',*,*,#2566,.F.);
#3407=ORIENTED_EDGE('',*,*,#2571,.T.);
#3408=ORIENTED_EDGE('',*,*,#2572,.T.);
#3409=ORIENTED_EDGE('',*,*,#2573,.T.);
#3410=ORIENTED_EDGE('',*,*,#2569,.F.);
#3411=ORIENTED_EDGE('',*,*,#2574,.T.);
#3412=ORIENTED_EDGE('',*,*,#2575,.T.);
#3413=ORIENTED_EDGE('',*,*,#2576,.T.);
#3414=ORIENTED_EDGE('',*,*,#2572,.F.);
#3415=ORIENTED_EDGE('',*,*,#2577,.T.);
#3416=ORIENTED_EDGE('',*,*,#2564,.T.);
#3417=ORIENTED_EDGE('',*,*,#2578,.T.);
#3418=ORIENTED_EDGE('',*,*,#2575,.F.);
#3419=ORIENTED_EDGE('',*,*,#2577,.F.);
#3420=ORIENTED_EDGE('',*,*,#2574,.F.);
#3421=ORIENTED_EDGE('',*,*,#2571,.F.);
#3422=ORIENTED_EDGE('',*,*,#2568,.F.);
#3423=ORIENTED_EDGE('',*,*,#2565,.F.);
#3424=ORIENTED_EDGE('',*,*,#2561,.F.);
#3425=ORIENTED_EDGE('',*,*,#2578,.F.);
#3426=ORIENTED_EDGE('',*,*,#2563,.F.);
#3427=ORIENTED_EDGE('',*,*,#2567,.F.);
#3428=ORIENTED_EDGE('',*,*,#2570,.F.);
#3429=ORIENTED_EDGE('',*,*,#2573,.F.);
#3430=ORIENTED_EDGE('',*,*,#2576,.F.);
#3431=ORIENTED_EDGE('',*,*,#2579,.F.);
#3432=ORIENTED_EDGE('',*,*,#2580,.F.);
#3433=ORIENTED_EDGE('',*,*,#2581,.T.);
#3434=ORIENTED_EDGE('',*,*,#2579,.T.);
#3435=ORIENTED_EDGE('',*,*,#2581,.F.);
#3436=ORIENTED_EDGE('',*,*,#2582,.F.);
#3437=ORIENTED_EDGE('',*,*,#2583,.T.);
#3438=ORIENTED_EDGE('',*,*,#2580,.T.);
#3439=ORIENTED_EDGE('',*,*,#2583,.F.);
#3440=ORIENTED_EDGE('',*,*,#2584,.F.);
#3441=ORIENTED_EDGE('',*,*,#2585,.T.);
#3442=ORIENTED_EDGE('',*,*,#2582,.T.);
#3443=ORIENTED_EDGE('',*,*,#2585,.F.);
#3444=ORIENTED_EDGE('',*,*,#2584,.T.);
#3445=ORIENTED_EDGE('',*,*,#2586,.F.);
#3446=ORIENTED_EDGE('',*,*,#2587,.F.);
#3447=ORIENTED_EDGE('',*,*,#2588,.T.);
#3448=ORIENTED_EDGE('',*,*,#2586,.T.);
#3449=ORIENTED_EDGE('',*,*,#2588,.F.);
#3450=ORIENTED_EDGE('',*,*,#2589,.F.);
#3451=ORIENTED_EDGE('',*,*,#2590,.T.);
#3452=ORIENTED_EDGE('',*,*,#2587,.T.);
#3453=ORIENTED_EDGE('',*,*,#2590,.F.);
#3454=ORIENTED_EDGE('',*,*,#2591,.F.);
#3455=ORIENTED_EDGE('',*,*,#2592,.T.);
#3456=ORIENTED_EDGE('',*,*,#2589,.T.);
#3457=ORIENTED_EDGE('',*,*,#2592,.F.);
#3458=ORIENTED_EDGE('',*,*,#2591,.T.);
#3459=ORIENTED_EDGE('',*,*,#2593,.T.);
#3460=ORIENTED_EDGE('',*,*,#2594,.T.);
#3461=ORIENTED_EDGE('',*,*,#2595,.T.);
#3462=ORIENTED_EDGE('',*,*,#2596,.F.);
#3463=ORIENTED_EDGE('',*,*,#2597,.T.);
#3464=ORIENTED_EDGE('',*,*,#2598,.T.);
#3465=ORIENTED_EDGE('',*,*,#2599,.T.);
#3466=ORIENTED_EDGE('',*,*,#2594,.F.);
#3467=ORIENTED_EDGE('',*,*,#2600,.T.);
#3468=ORIENTED_EDGE('',*,*,#2601,.T.);
#3469=ORIENTED_EDGE('',*,*,#2602,.T.);
#3470=ORIENTED_EDGE('',*,*,#2598,.F.);
#3471=ORIENTED_EDGE('',*,*,#2603,.T.);
#3472=ORIENTED_EDGE('',*,*,#2604,.T.);
#3473=ORIENTED_EDGE('',*,*,#2605,.T.);
#3474=ORIENTED_EDGE('',*,*,#2601,.F.);
#3475=ORIENTED_EDGE('',*,*,#2606,.T.);
#3476=ORIENTED_EDGE('',*,*,#2607,.T.);
#3477=ORIENTED_EDGE('',*,*,#2608,.T.);
#3478=ORIENTED_EDGE('',*,*,#2604,.F.);
#3479=ORIENTED_EDGE('',*,*,#2609,.T.);
#3480=ORIENTED_EDGE('',*,*,#2596,.T.);
#3481=ORIENTED_EDGE('',*,*,#2610,.T.);
#3482=ORIENTED_EDGE('',*,*,#2607,.F.);
#3483=ORIENTED_EDGE('',*,*,#2609,.F.);
#3484=ORIENTED_EDGE('',*,*,#2606,.F.);
#3485=ORIENTED_EDGE('',*,*,#2603,.F.);
#3486=ORIENTED_EDGE('',*,*,#2600,.F.);
#3487=ORIENTED_EDGE('',*,*,#2597,.F.);
#3488=ORIENTED_EDGE('',*,*,#2593,.F.);
#3489=ORIENTED_EDGE('',*,*,#2610,.F.);
#3490=ORIENTED_EDGE('',*,*,#2595,.F.);
#3491=ORIENTED_EDGE('',*,*,#2599,.F.);
#3492=ORIENTED_EDGE('',*,*,#2602,.F.);
#3493=ORIENTED_EDGE('',*,*,#2605,.F.);
#3494=ORIENTED_EDGE('',*,*,#2608,.F.);
#3495=ORIENTED_EDGE('',*,*,#2611,.F.);
#3496=ORIENTED_EDGE('',*,*,#2612,.T.);
#3497=ORIENTED_EDGE('',*,*,#2613,.F.);
#3498=ORIENTED_EDGE('',*,*,#2614,.T.);
#3499=ORIENTED_EDGE('',*,*,#2615,.F.);
#3500=ORIENTED_EDGE('',*,*,#2614,.F.);
#3501=ORIENTED_EDGE('',*,*,#2616,.F.);
#3502=ORIENTED_EDGE('',*,*,#2617,.F.);
#3503=ORIENTED_EDGE('',*,*,#2618,.F.);
#3504=ORIENTED_EDGE('',*,*,#2617,.T.);
#3505=ORIENTED_EDGE('',*,*,#2619,.T.);
#3506=ORIENTED_EDGE('',*,*,#2620,.T.);
#3507=ORIENTED_EDGE('',*,*,#2616,.T.);
#3508=ORIENTED_EDGE('',*,*,#2613,.T.);
#3509=ORIENTED_EDGE('',*,*,#2621,.T.);
#3510=ORIENTED_EDGE('',*,*,#2619,.F.);
#3511=ORIENTED_EDGE('',*,*,#2622,.F.);
#3512=ORIENTED_EDGE('',*,*,#2620,.F.);
#3513=ORIENTED_EDGE('',*,*,#2621,.F.);
#3514=ORIENTED_EDGE('',*,*,#2612,.F.);
#3515=ORIENTED_EDGE('',*,*,#2623,.T.);
#3516=ORIENTED_EDGE('',*,*,#2624,.F.);
#3517=ORIENTED_EDGE('',*,*,#2625,.F.);
#3518=ORIENTED_EDGE('',*,*,#2626,.F.);
#3519=ORIENTED_EDGE('',*,*,#2623,.F.);
#3520=ORIENTED_EDGE('',*,*,#2627,.T.);
#3521=ORIENTED_EDGE('',*,*,#2625,.T.);
#3522=ORIENTED_EDGE('',*,*,#2627,.F.);
#3523=ORIENTED_EDGE('',*,*,#2626,.T.);
#3524=ORIENTED_EDGE('',*,*,#2628,.T.);
#3525=ORIENTED_EDGE('',*,*,#2629,.T.);
#3526=ORIENTED_EDGE('',*,*,#2628,.F.);
#3527=ORIENTED_EDGE('',*,*,#2618,.T.);
#3528=ORIENTED_EDGE('',*,*,#2622,.T.);
#3529=ORIENTED_EDGE('',*,*,#2611,.T.);
#3530=ORIENTED_EDGE('',*,*,#2615,.T.);
#3531=ORIENTED_EDGE('',*,*,#2630,.F.);
#3532=ORIENTED_EDGE('',*,*,#2631,.T.);
#3533=ORIENTED_EDGE('',*,*,#2624,.T.);
#3534=ORIENTED_EDGE('',*,*,#2631,.F.);
#3535=ORIENTED_EDGE('',*,*,#2630,.T.);
#3536=ORIENTED_EDGE('',*,*,#2629,.F.);
#3537=ORIENTED_EDGE('',*,*,#2632,.F.);
#3538=ORIENTED_EDGE('',*,*,#2633,.T.);
#3539=ORIENTED_EDGE('',*,*,#2634,.T.);
#3540=ORIENTED_EDGE('',*,*,#2633,.F.);
#3541=ORIENTED_EDGE('',*,*,#2635,.F.);
#3542=ORIENTED_EDGE('',*,*,#2636,.T.);
#3543=ORIENTED_EDGE('',*,*,#2637,.T.);
#3544=ORIENTED_EDGE('',*,*,#2636,.F.);
#3545=ORIENTED_EDGE('',*,*,#2635,.T.);
#3546=ORIENTED_EDGE('',*,*,#2632,.T.);
#3547=ORIENTED_EDGE('',*,*,#2637,.F.);
#3548=ORIENTED_EDGE('',*,*,#2634,.F.);
#3549=ORIENTED_EDGE('',*,*,#2638,.F.);
#3550=ORIENTED_EDGE('',*,*,#2639,.T.);
#3551=ORIENTED_EDGE('',*,*,#2640,.F.);
#3552=ORIENTED_EDGE('',*,*,#2641,.F.);
#3553=ORIENTED_EDGE('',*,*,#2642,.T.);
#3554=ORIENTED_EDGE('',*,*,#2643,.F.);
#3555=ORIENTED_EDGE('',*,*,#2644,.F.);
#3556=ORIENTED_EDGE('',*,*,#2642,.F.);
#3557=ORIENTED_EDGE('',*,*,#2645,.F.);
#3558=ORIENTED_EDGE('',*,*,#2646,.F.);
#3559=ORIENTED_EDGE('',*,*,#2639,.F.);
#3560=ORIENTED_EDGE('',*,*,#2647,.F.);
#3561=ORIENTED_EDGE('',*,*,#2645,.T.);
#3562=ORIENTED_EDGE('',*,*,#2641,.T.);
#3563=ORIENTED_EDGE('',*,*,#2648,.F.);
#3564=ORIENTED_EDGE('',*,*,#2649,.T.);
#3565=ORIENTED_EDGE('',*,*,#2650,.T.);
#3566=ORIENTED_EDGE('',*,*,#2649,.F.);
#3567=ORIENTED_EDGE('',*,*,#2646,.T.);
#3568=ORIENTED_EDGE('',*,*,#2647,.T.);
#3569=ORIENTED_EDGE('',*,*,#2640,.T.);
#3570=ORIENTED_EDGE('',*,*,#2638,.T.);
#3571=ORIENTED_EDGE('',*,*,#2651,.F.);
#3572=ORIENTED_EDGE('',*,*,#2652,.T.);
#3573=ORIENTED_EDGE('',*,*,#2653,.T.);
#3574=ORIENTED_EDGE('',*,*,#2652,.F.);
#3575=ORIENTED_EDGE('',*,*,#2643,.T.);
#3576=ORIENTED_EDGE('',*,*,#2644,.T.);
#3577=ORIENTED_EDGE('',*,*,#2651,.T.);
#3578=ORIENTED_EDGE('',*,*,#2648,.T.);
#3579=ORIENTED_EDGE('',*,*,#2653,.F.);
#3580=ORIENTED_EDGE('',*,*,#2650,.F.);
#3581=ORIENTED_EDGE('',*,*,#2654,.F.);
#3582=ORIENTED_EDGE('',*,*,#2655,.T.);
#3583=ORIENTED_EDGE('',*,*,#2656,.F.);
#3584=ORIENTED_EDGE('',*,*,#2657,.F.);
#3585=ORIENTED_EDGE('',*,*,#2658,.T.);
#3586=ORIENTED_EDGE('',*,*,#2659,.F.);
#3587=ORIENTED_EDGE('',*,*,#2660,.F.);
#3588=ORIENTED_EDGE('',*,*,#2658,.F.);
#3589=ORIENTED_EDGE('',*,*,#2661,.F.);
#3590=ORIENTED_EDGE('',*,*,#2662,.F.);
#3591=ORIENTED_EDGE('',*,*,#2655,.F.);
#3592=ORIENTED_EDGE('',*,*,#2663,.F.);
#3593=ORIENTED_EDGE('',*,*,#2661,.T.);
#3594=ORIENTED_EDGE('',*,*,#2657,.T.);
#3595=ORIENTED_EDGE('',*,*,#2664,.F.);
#3596=ORIENTED_EDGE('',*,*,#2665,.T.);
#3597=ORIENTED_EDGE('',*,*,#2666,.F.);
#3598=ORIENTED_EDGE('',*,*,#2667,.F.);
#3599=ORIENTED_EDGE('',*,*,#2668,.F.);
#3600=ORIENTED_EDGE('',*,*,#2669,.T.);
#3601=ORIENTED_EDGE('',*,*,#2670,.F.);
#3602=ORIENTED_EDGE('',*,*,#2665,.F.);
#3603=ORIENTED_EDGE('',*,*,#2671,.F.);
#3604=ORIENTED_EDGE('',*,*,#2672,.F.);
#3605=ORIENTED_EDGE('',*,*,#2673,.F.);
#3606=ORIENTED_EDGE('',*,*,#2669,.F.);
#3607=ORIENTED_EDGE('',*,*,#2674,.T.);
#3608=ORIENTED_EDGE('',*,*,#2666,.T.);
#3609=ORIENTED_EDGE('',*,*,#2670,.T.);
#3610=ORIENTED_EDGE('',*,*,#2673,.T.);
#3611=ORIENTED_EDGE('',*,*,#2675,.T.);
#3612=ORIENTED_EDGE('',*,*,#2667,.T.);
#3613=ORIENTED_EDGE('',*,*,#2675,.F.);
#3614=ORIENTED_EDGE('',*,*,#2672,.T.);
#3615=ORIENTED_EDGE('',*,*,#2676,.T.);
#3616=ORIENTED_EDGE('',*,*,#2662,.T.);
#3617=ORIENTED_EDGE('',*,*,#2663,.T.);
#3618=ORIENTED_EDGE('',*,*,#2656,.T.);
#3619=ORIENTED_EDGE('',*,*,#2654,.T.);
#3620=ORIENTED_EDGE('',*,*,#2677,.F.);
#3621=ORIENTED_EDGE('',*,*,#2678,.T.);
#3622=ORIENTED_EDGE('',*,*,#2679,.F.);
#3623=ORIENTED_EDGE('',*,*,#2678,.F.);
#3624=ORIENTED_EDGE('',*,*,#2680,.F.);
#3625=ORIENTED_EDGE('',*,*,#2681,.T.);
#3626=ORIENTED_EDGE('',*,*,#2682,.F.);
#3627=ORIENTED_EDGE('',*,*,#2681,.F.);
#3628=ORIENTED_EDGE('',*,*,#2683,.F.);
#3629=ORIENTED_EDGE('',*,*,#2684,.T.);
#3630=ORIENTED_EDGE('',*,*,#2685,.F.);
#3631=ORIENTED_EDGE('',*,*,#2684,.F.);
#3632=ORIENTED_EDGE('',*,*,#2686,.F.);
#3633=ORIENTED_EDGE('',*,*,#2687,.T.);
#3634=ORIENTED_EDGE('',*,*,#2688,.F.);
#3635=ORIENTED_EDGE('',*,*,#2687,.F.);
#3636=ORIENTED_EDGE('',*,*,#2689,.T.);
#3637=ORIENTED_EDGE('',*,*,#2690,.F.);
#3638=ORIENTED_EDGE('',*,*,#2688,.T.);
#3639=ORIENTED_EDGE('',*,*,#2685,.T.);
#3640=ORIENTED_EDGE('',*,*,#2682,.T.);
#3641=ORIENTED_EDGE('',*,*,#2679,.T.);
#3642=ORIENTED_EDGE('',*,*,#2689,.F.);
#3643=ORIENTED_EDGE('',*,*,#2691,.T.);
#3644=ORIENTED_EDGE('',*,*,#2692,.T.);
#3645=ORIENTED_EDGE('',*,*,#2691,.F.);
#3646=ORIENTED_EDGE('',*,*,#2674,.F.);
#3647=ORIENTED_EDGE('',*,*,#2693,.T.);
#3648=ORIENTED_EDGE('',*,*,#2690,.T.);
#3649=ORIENTED_EDGE('',*,*,#2693,.F.);
#3650=ORIENTED_EDGE('',*,*,#2659,.T.);
#3651=ORIENTED_EDGE('',*,*,#2660,.T.);
#3652=ORIENTED_EDGE('',*,*,#2692,.F.);
#3653=ORIENTED_EDGE('',*,*,#2664,.T.);
#3654=ORIENTED_EDGE('',*,*,#2676,.F.);
#3655=ORIENTED_EDGE('',*,*,#2671,.T.);
#3656=ORIENTED_EDGE('',*,*,#2668,.T.);
#3657=ORIENTED_EDGE('',*,*,#2686,.T.);
#3658=ORIENTED_EDGE('',*,*,#2683,.T.);
#3659=ORIENTED_EDGE('',*,*,#2680,.T.);
#3660=ORIENTED_EDGE('',*,*,#2677,.T.);
#3661=ORIENTED_EDGE('',*,*,#2694,.F.);
#3662=ORIENTED_EDGE('',*,*,#2695,.F.);
#3663=ORIENTED_EDGE('',*,*,#2696,.F.);
#3664=ORIENTED_EDGE('',*,*,#2697,.F.);
#3665=ORIENTED_EDGE('',*,*,#2698,.F.);
#3666=ORIENTED_EDGE('',*,*,#2699,.F.);
#3667=ORIENTED_EDGE('',*,*,#2700,.F.);
#3668=ORIENTED_EDGE('',*,*,#2701,.F.);
#3669=ORIENTED_EDGE('',*,*,#2698,.T.);
#3670=ORIENTED_EDGE('',*,*,#2702,.T.);
#3671=ORIENTED_EDGE('',*,*,#2703,.T.);
#3672=ORIENTED_EDGE('',*,*,#2704,.T.);
#3673=ORIENTED_EDGE('',*,*,#2697,.T.);
#3674=ORIENTED_EDGE('',*,*,#2705,.F.);
#3675=ORIENTED_EDGE('',*,*,#2706,.T.);
#3676=ORIENTED_EDGE('',*,*,#2702,.F.);
#3677=ORIENTED_EDGE('',*,*,#2696,.T.);
#3678=ORIENTED_EDGE('',*,*,#2707,.T.);
#3679=ORIENTED_EDGE('',*,*,#2708,.T.);
#3680=ORIENTED_EDGE('',*,*,#2705,.T.);
#3681=ORIENTED_EDGE('',*,*,#2695,.T.);
#3682=ORIENTED_EDGE('',*,*,#2709,.F.);
#3683=ORIENTED_EDGE('',*,*,#2710,.T.);
#3684=ORIENTED_EDGE('',*,*,#2707,.F.);
#3685=ORIENTED_EDGE('',*,*,#2711,.F.);
#3686=ORIENTED_EDGE('',*,*,#2712,.F.);
#3687=ORIENTED_EDGE('',*,*,#2703,.F.);
#3688=ORIENTED_EDGE('',*,*,#2706,.F.);
#3689=ORIENTED_EDGE('',*,*,#2708,.F.);
#3690=ORIENTED_EDGE('',*,*,#2710,.F.);
#3691=ORIENTED_EDGE('',*,*,#2713,.F.);
#3692=ORIENTED_EDGE('',*,*,#2714,.F.);
#3693=ORIENTED_EDGE('',*,*,#2699,.T.);
#3694=ORIENTED_EDGE('',*,*,#2704,.F.);
#3695=ORIENTED_EDGE('',*,*,#2712,.T.);
#3696=ORIENTED_EDGE('',*,*,#2715,.F.);
#3697=ORIENTED_EDGE('',*,*,#2694,.T.);
#3698=ORIENTED_EDGE('',*,*,#2716,.T.);
#3699=ORIENTED_EDGE('',*,*,#2713,.T.);
#3700=ORIENTED_EDGE('',*,*,#2709,.T.);
#3701=ORIENTED_EDGE('',*,*,#2700,.T.);
#3702=ORIENTED_EDGE('',*,*,#2715,.T.);
#3703=ORIENTED_EDGE('',*,*,#2711,.T.);
#3704=ORIENTED_EDGE('',*,*,#2717,.T.);
#3705=ORIENTED_EDGE('',*,*,#2701,.T.);
#3706=ORIENTED_EDGE('',*,*,#2717,.F.);
#3707=ORIENTED_EDGE('',*,*,#2714,.T.);
#3708=ORIENTED_EDGE('',*,*,#2716,.F.);
#3709=ORIENTED_EDGE('',*,*,#2718,.F.);
#3710=ORIENTED_EDGE('',*,*,#2719,.T.);
#3711=ORIENTED_EDGE('',*,*,#2720,.T.);
#3712=ORIENTED_EDGE('',*,*,#2721,.F.);
#3713=ORIENTED_EDGE('',*,*,#2722,.F.);
#3714=ORIENTED_EDGE('',*,*,#2723,.T.);
#3715=ORIENTED_EDGE('',*,*,#2724,.T.);
#3716=ORIENTED_EDGE('',*,*,#2719,.F.);
#3717=ORIENTED_EDGE('',*,*,#2725,.F.);
#3718=ORIENTED_EDGE('',*,*,#2726,.T.);
#3719=ORIENTED_EDGE('',*,*,#2727,.T.);
#3720=ORIENTED_EDGE('',*,*,#2723,.F.);
#3721=ORIENTED_EDGE('',*,*,#2728,.F.);
#3722=ORIENTED_EDGE('',*,*,#2729,.T.);
#3723=ORIENTED_EDGE('',*,*,#2730,.T.);
#3724=ORIENTED_EDGE('',*,*,#2726,.F.);
#3725=ORIENTED_EDGE('',*,*,#2731,.F.);
#3726=ORIENTED_EDGE('',*,*,#2732,.T.);
#3727=ORIENTED_EDGE('',*,*,#2733,.T.);
#3728=ORIENTED_EDGE('',*,*,#2729,.F.);
#3729=ORIENTED_EDGE('',*,*,#2734,.F.);
#3730=ORIENTED_EDGE('',*,*,#2721,.T.);
#3731=ORIENTED_EDGE('',*,*,#2735,.T.);
#3732=ORIENTED_EDGE('',*,*,#2732,.F.);
#3733=ORIENTED_EDGE('',*,*,#2735,.F.);
#3734=ORIENTED_EDGE('',*,*,#2720,.F.);
#3735=ORIENTED_EDGE('',*,*,#2724,.F.);
#3736=ORIENTED_EDGE('',*,*,#2727,.F.);
#3737=ORIENTED_EDGE('',*,*,#2730,.F.);
#3738=ORIENTED_EDGE('',*,*,#2733,.F.);
#3739=ORIENTED_EDGE('',*,*,#2736,.F.);
#3740=ORIENTED_EDGE('',*,*,#2718,.T.);
#3741=ORIENTED_EDGE('',*,*,#2734,.T.);
#3742=ORIENTED_EDGE('',*,*,#2731,.T.);
#3743=ORIENTED_EDGE('',*,*,#2728,.T.);
#3744=ORIENTED_EDGE('',*,*,#2725,.T.);
#3745=ORIENTED_EDGE('',*,*,#2722,.T.);
#3746=ORIENTED_EDGE('',*,*,#2737,.F.);
#3747=ORIENTED_EDGE('',*,*,#2738,.T.);
#3748=ORIENTED_EDGE('',*,*,#2736,.T.);
#3749=ORIENTED_EDGE('',*,*,#2738,.F.);
#3750=ORIENTED_EDGE('',*,*,#2739,.F.);
#3751=ORIENTED_EDGE('',*,*,#2740,.T.);
#3752=ORIENTED_EDGE('',*,*,#2737,.T.);
#3753=ORIENTED_EDGE('',*,*,#2740,.F.);
#3754=ORIENTED_EDGE('',*,*,#2741,.F.);
#3755=ORIENTED_EDGE('',*,*,#2742,.T.);
#3756=ORIENTED_EDGE('',*,*,#2739,.T.);
#3757=ORIENTED_EDGE('',*,*,#2742,.F.);
#3758=ORIENTED_EDGE('',*,*,#2741,.T.);
#3759=CYLINDRICAL_SURFACE('',#4351,0.25);
#3760=CYLINDRICAL_SURFACE('',#4354,0.25);
#3761=CYLINDRICAL_SURFACE('',#4357,0.25);
#3762=CYLINDRICAL_SURFACE('',#4360,0.25);
#3763=CYLINDRICAL_SURFACE('',#4370,0.165);
#3764=CYLINDRICAL_SURFACE('',#4374,0.165);
#3765=CYLINDRICAL_SURFACE('',#4378,0.165);
#3766=CYLINDRICAL_SURFACE('',#4382,0.165);
#3767=CYLINDRICAL_SURFACE('',#4386,0.165);
#3768=CYLINDRICAL_SURFACE('',#4390,0.165);
#3769=CYLINDRICAL_SURFACE('',#4394,0.165);
#3770=CYLINDRICAL_SURFACE('',#4398,0.165);
#3771=CYLINDRICAL_SURFACE('',#4402,0.33);
#3772=CYLINDRICAL_SURFACE('',#4405,0.33);
#3773=CYLINDRICAL_SURFACE('',#4408,0.33);
#3774=CYLINDRICAL_SURFACE('',#4411,0.33);
#3775=CYLINDRICAL_SURFACE('',#4440,2.35);
#3776=CYLINDRICAL_SURFACE('',#4443,3.5);
#3777=CYLINDRICAL_SURFACE('',#4449,1.75);
#3778=CYLINDRICAL_SURFACE('',#4452,2.34);
#3779=CYLINDRICAL_SURFACE('',#4458,0.225);
#3780=CYLINDRICAL_SURFACE('',#4461,0.225);
#3781=CYLINDRICAL_SURFACE('',#4464,0.225);
#3782=CYLINDRICAL_SURFACE('',#4467,0.225);
#3783=CYLINDRICAL_SURFACE('',#4470,2.34);
#3784=CYLINDRICAL_SURFACE('',#4475,1.8);
#3785=CYLINDRICAL_SURFACE('',#4480,1.6);
#3786=CYLINDRICAL_SURFACE('',#4481,3.5);
#3787=CYLINDRICAL_SURFACE('',#4487,1.);
#3788=CYLINDRICAL_SURFACE('',#4490,1.8);
#3789=CYLINDRICAL_SURFACE('',#4496,0.4);
#3790=CYLINDRICAL_SURFACE('',#4501,0.4);
#3791=CYLINDRICAL_SURFACE('',#4506,0.4);
#3792=CYLINDRICAL_SURFACE('',#4511,0.4);
#3793=CYLINDRICAL_SURFACE('',#4516,0.225);
#3794=CYLINDRICAL_SURFACE('',#4518,0.225);
#3795=CYLINDRICAL_SURFACE('',#4520,0.225);
#3796=CYLINDRICAL_SURFACE('',#4522,0.225);
#3797=CYLINDRICAL_SURFACE('',#4527,1.8);
#3798=CYLINDRICAL_SURFACE('',#4529,2.34);
#3799=CYLINDRICAL_SURFACE('',#4533,2.);
#3800=CYLINDRICAL_SURFACE('',#4536,3.5);
#3801=CYLINDRICAL_SURFACE('',#4563,1.63531);
#3802=CYLINDRICAL_SURFACE('',#4565,1.);
#3803=CYLINDRICAL_SURFACE('',#4571,1.63531);
#3804=CYLINDRICAL_SURFACE('',#4583,1.71469);
#3805=CYLINDRICAL_SURFACE('',#4590,2.35);
#3806=CYLINDRICAL_SURFACE('',#4595,1.71469);
#3807=CYLINDRICAL_SURFACE('',#4617,1.706752);
#3808=CYLINDRICAL_SURFACE('',#4657,1.643248);
#3809=CYLINDRICAL_SURFACE('',#4671,1.70469);
#3810=CYLINDRICAL_SURFACE('',#4675,1.65031);
#3811=CYLINDRICAL_SURFACE('',#4679,1.70469);
#3812=CYLINDRICAL_SURFACE('',#4683,1.65031);
#3813=CYLINDRICAL_SURFACE('',#4694,0.5);
#3814=CYLINDRICAL_SURFACE('',#4702,0.2942);
#3815=CYLINDRICAL_SURFACE('',#4720,0.35);
#3816=CYLINDRICAL_SURFACE('',#4728,0.1954);
#3817=CYLINDRICAL_SURFACE('',#4778,1.2);
#3818=CYLINDRICAL_SURFACE('',#4779,1.);
#3819=CYLINDRICAL_SURFACE('',#4781,1.);
#3820=CYLINDRICAL_SURFACE('',#4786,1.01);
#3821=CYLINDRICAL_SURFACE('',#4789,1.35);
#3822=CYLINDRICAL_SURFACE('',#4797,0.21);
#3823=CYLINDRICAL_SURFACE('',#4801,1.005);
#3824=CYLINDRICAL_SURFACE('',#4804,1.5);
#3825=CYLINDRICAL_SURFACE('',#4812,0.21);
#3826=CYLINDRICAL_SURFACE('',#4822,1.);
#3827=CYLINDRICAL_SURFACE('',#4824,0.33);
#3828=CYLINDRICAL_SURFACE('',#4827,0.33);
#3829=CYLINDRICAL_SURFACE('',#4830,0.33);
#3830=CYLINDRICAL_SURFACE('',#4833,0.33);
#3831=CYLINDRICAL_SURFACE('',#4839,3.5);
#3832=CYLINDRICAL_SURFACE('',#4841,1.6);
#3833=CYLINDRICAL_SURFACE('',#4866,0.24505);
#3834=ADVANCED_FACE('',(#552),#3759,.F.);
#3835=ADVANCED_FACE('',(#553),#3760,.F.);
#3836=ADVANCED_FACE('',(#554),#3761,.F.);
#3837=ADVANCED_FACE('',(#555),#3762,.F.);
#3838=ADVANCED_FACE('',(#556),#408,.T.);
#3839=ADVANCED_FACE('',(#557),#409,.T.);
#3840=ADVANCED_FACE('',(#558),#410,.T.);
#3841=ADVANCED_FACE('',(#559),#411,.T.);
#3842=ADVANCED_FACE('',(#560,#315,#316,#317,#318),#412,.T.);
#3843=ADVANCED_FACE('',(#561,#319,#320,#321,#322),#413,.F.);
#3844=ADVANCED_FACE('',(#562),#3763,.F.);
#3845=ADVANCED_FACE('',(#563),#414,.T.);
#3846=ADVANCED_FACE('',(#564),#3764,.F.);
#3847=ADVANCED_FACE('',(#565),#415,.T.);
#3848=ADVANCED_FACE('',(#566),#3765,.F.);
#3849=ADVANCED_FACE('',(#567),#416,.T.);
#3850=ADVANCED_FACE('',(#568),#3766,.F.);
#3851=ADVANCED_FACE('',(#569),#417,.T.);
#3852=ADVANCED_FACE('',(#570),#3767,.F.);
#3853=ADVANCED_FACE('',(#571),#418,.F.);
#3854=ADVANCED_FACE('',(#572),#3768,.F.);
#3855=ADVANCED_FACE('',(#573),#419,.F.);
#3856=ADVANCED_FACE('',(#574),#3769,.F.);
#3857=ADVANCED_FACE('',(#575),#420,.F.);
#3858=ADVANCED_FACE('',(#576),#3770,.F.);
#3859=ADVANCED_FACE('',(#577),#421,.F.);
#3860=ADVANCED_FACE('',(#578),#3771,.F.);
#3861=ADVANCED_FACE('',(#579),#3772,.F.);
#3862=ADVANCED_FACE('',(#580),#3773,.F.);
#3863=ADVANCED_FACE('',(#581),#3774,.F.);
#3864=ADVANCED_FACE('',(#582),#422,.T.);
#3865=ADVANCED_FACE('',(#583),#423,.T.);
#3866=ADVANCED_FACE('',(#584),#424,.F.);
#3867=ADVANCED_FACE('',(#585),#425,.F.);
#3868=ADVANCED_FACE('',(#586,#323),#426,.T.);
#3869=ADVANCED_FACE('',(#587,#324),#427,.T.);
#3870=ADVANCED_FACE('',(#588),#428,.T.);
#3871=ADVANCED_FACE('',(#589,#325,#326),#429,.T.);
#3872=ADVANCED_FACE('',(#590),#430,.T.);
#3873=ADVANCED_FACE('',(#591),#431,.T.);
#3874=ADVANCED_FACE('',(#592),#432,.T.);
#3875=ADVANCED_FACE('',(#593),#433,.F.);
#3876=ADVANCED_FACE('',(#594),#434,.F.);
#3877=ADVANCED_FACE('',(#595,#327),#435,.T.);
#3878=ADVANCED_FACE('',(#596,#328),#436,.T.);
#3879=ADVANCED_FACE('',(#597),#437,.T.);
#3880=ADVANCED_FACE('',(#598,#329,#330),#438,.T.);
#3881=ADVANCED_FACE('',(#599),#439,.T.);
#3882=ADVANCED_FACE('',(#600),#3775,.F.);
#3883=ADVANCED_FACE('',(#601,#331,#332),#3776,.T.);
#3884=ADVANCED_FACE('',(#602,#333,#334,#335,#336,#337),#440,.T.);
#3885=ADVANCED_FACE('',(#603,#338,#339,#340,#341,#342),#441,.F.);
#3886=ADVANCED_FACE('',(#604),#3777,.F.);
#3887=ADVANCED_FACE('',(#605),#3778,.T.);
#3888=ADVANCED_FACE('',(#606,#343),#442,.T.);
#3889=ADVANCED_FACE('',(#607,#344),#443,.F.);
#3890=ADVANCED_FACE('',(#608),#3779,.F.);
#3891=ADVANCED_FACE('',(#609),#3780,.F.);
#3892=ADVANCED_FACE('',(#610),#3781,.F.);
#3893=ADVANCED_FACE('',(#611),#3782,.F.);
#3894=ADVANCED_FACE('',(#612),#3783,.T.);
#3895=ADVANCED_FACE('',(#613,#345),#444,.T.);
#3896=ADVANCED_FACE('',(#614),#3784,.F.);
#3897=ADVANCED_FACE('',(#615,#346),#445,.F.);
#3898=ADVANCED_FACE('',(#616),#3785,.F.);
#3899=ADVANCED_FACE('',(#617),#3786,.T.);
#3900=ADVANCED_FACE('',(#618,#347,#348,#349,#350,#351),#446,.T.);
#3901=ADVANCED_FACE('',(#619,#352,#353,#354,#355,#356),#447,.F.);
#3902=ADVANCED_FACE('',(#620),#3787,.F.);
#3903=ADVANCED_FACE('',(#621),#3788,.T.);
#3904=ADVANCED_FACE('',(#622,#357),#448,.T.);
#3905=ADVANCED_FACE('',(#623,#358),#449,.F.);
#3906=ADVANCED_FACE('',(#624),#3789,.F.);
#3907=ADVANCED_FACE('',(#625,#359),#450,.T.);
#3908=ADVANCED_FACE('',(#626),#3790,.F.);
#3909=ADVANCED_FACE('',(#627,#360),#451,.T.);
#3910=ADVANCED_FACE('',(#628),#3791,.F.);
#3911=ADVANCED_FACE('',(#629,#361),#452,.T.);
#3912=ADVANCED_FACE('',(#630),#3792,.F.);
#3913=ADVANCED_FACE('',(#631,#362),#453,.T.);
#3914=ADVANCED_FACE('',(#632),#3793,.F.);
#3915=ADVANCED_FACE('',(#633),#3794,.F.);
#3916=ADVANCED_FACE('',(#634),#3795,.F.);
#3917=ADVANCED_FACE('',(#635),#3796,.F.);
#3918=ADVANCED_FACE('',(#636,#363),#454,.T.);
#3919=ADVANCED_FACE('',(#637),#3797,.F.);
#3920=ADVANCED_FACE('',(#638),#3798,.T.);
#3921=ADVANCED_FACE('',(#639,#364),#455,.F.);
#3922=ADVANCED_FACE('',(#640),#3799,.F.);
#3923=ADVANCED_FACE('',(#641),#456,.F.);
#3924=ADVANCED_FACE('',(#642),#3800,.T.);
#3925=ADVANCED_FACE('',(#643,#365,#366,#367,#368),#457,.T.);
#3926=ADVANCED_FACE('',(#644,#369,#370,#371,#372,#373),#458,.F.);
#3927=ADVANCED_FACE('',(#645),#459,.T.);
#3928=ADVANCED_FACE('',(#646),#460,.T.);
#3929=ADVANCED_FACE('',(#647),#461,.T.);
#3930=ADVANCED_FACE('',(#648),#462,.T.);
#3931=ADVANCED_FACE('',(#649),#463,.T.);
#3932=ADVANCED_FACE('',(#650),#464,.F.);
#3933=ADVANCED_FACE('',(#651),#465,.T.);
#3934=ADVANCED_FACE('',(#652),#466,.T.);
#3935=ADVANCED_FACE('',(#653),#467,.T.);
#3936=ADVANCED_FACE('',(#654),#468,.T.);
#3937=ADVANCED_FACE('',(#655),#469,.T.);
#3938=ADVANCED_FACE('',(#656),#470,.F.);
#3939=ADVANCED_FACE('',(#657),#215,.F.);
#3940=ADVANCED_FACE('',(#658),#3801,.T.);
#3941=ADVANCED_FACE('',(#659),#3802,.F.);
#3942=ADVANCED_FACE('',(#660),#201,.F.);
#3943=ADVANCED_FACE('',(#661,#374),#471,.T.);
#3944=ADVANCED_FACE('',(#662),#3803,.T.);
#3945=ADVANCED_FACE('',(#663,#375),#472,.T.);
#3946=ADVANCED_FACE('',(#664),#202,.F.);
#3947=ADVANCED_FACE('',(#665),#216,.F.);
#3948=ADVANCED_FACE('',(#666),#3804,.F.);
#3949=ADVANCED_FACE('',(#667,#376),#473,.T.);
#3950=ADVANCED_FACE('',(#668),#203,.T.);
#3951=ADVANCED_FACE('',(#669),#3805,.T.);
#3952=ADVANCED_FACE('',(#670),#204,.T.);
#3953=ADVANCED_FACE('',(#671,#377),#474,.T.);
#3954=ADVANCED_FACE('',(#672),#3806,.F.);
#3955=ADVANCED_FACE('',(#673),#185,.T.);
#3956=ADVANCED_FACE('',(#674),#186,.T.);
#3957=ADVANCED_FACE('',(#675),#187,.T.);
#3958=ADVANCED_FACE('',(#676),#188,.T.);
#3959=ADVANCED_FACE('',(#677),#189,.T.);
#3960=ADVANCED_FACE('',(#678),#190,.T.);
#3961=ADVANCED_FACE('',(#679),#191,.T.);
#3962=ADVANCED_FACE('',(#680),#192,.T.);
#3963=ADVANCED_FACE('',(#681),#193,.F.);
#3964=ADVANCED_FACE('',(#682),#3807,.T.);
#3965=ADVANCED_FACE('',(#683),#475,.T.);
#3966=ADVANCED_FACE('',(#684),#194,.F.);
#3967=ADVANCED_FACE('',(#685),#476,.T.);
#3968=ADVANCED_FACE('',(#686),#195,.F.);
#3969=ADVANCED_FACE('',(#687),#477,.T.);
#3970=ADVANCED_FACE('',(#688),#196,.F.);
#3971=ADVANCED_FACE('',(#689),#478,.T.);
#3972=ADVANCED_FACE('',(#690),#197,.F.);
#3973=ADVANCED_FACE('',(#691),#479,.T.);
#3974=ADVANCED_FACE('',(#692),#198,.F.);
#3975=ADVANCED_FACE('',(#693),#480,.T.);
#3976=ADVANCED_FACE('',(#694),#199,.F.);
#3977=ADVANCED_FACE('',(#695),#3808,.F.);
#3978=ADVANCED_FACE('',(#696),#481,.T.);
#3979=ADVANCED_FACE('',(#697),#200,.F.);
#3980=ADVANCED_FACE('',(#698,#378),#482,.T.);
#3981=ADVANCED_FACE('',(#699),#483,.T.);
#3982=ADVANCED_FACE('',(#700,#379),#484,.T.);
#3983=ADVANCED_FACE('',(#701),#3809,.T.);
#3984=ADVANCED_FACE('',(#702,#380),#485,.T.);
#3985=ADVANCED_FACE('',(#703),#3810,.F.);
#3986=ADVANCED_FACE('',(#704,#381),#486,.T.);
#3987=ADVANCED_FACE('',(#705),#3811,.T.);
#3988=ADVANCED_FACE('',(#706,#382),#487,.T.);
#3989=ADVANCED_FACE('',(#707),#3812,.F.);
#3990=ADVANCED_FACE('',(#708),#488,.T.);
#3991=ADVANCED_FACE('',(#709),#205,.T.);
#3992=ADVANCED_FACE('',(#710),#3813,.T.);
#3993=ADVANCED_FACE('',(#711),#206,.T.);
#3994=ADVANCED_FACE('',(#712,#383),#489,.T.);
#3995=ADVANCED_FACE('',(#713),#207,.T.);
#3996=ADVANCED_FACE('',(#714),#3814,.T.);
#3997=ADVANCED_FACE('',(#715),#208,.T.);
#3998=ADVANCED_FACE('',(#716),#490,.T.);
#3999=ADVANCED_FACE('',(#717),#491,.F.);
#4000=ADVANCED_FACE('',(#718),#492,.F.);
#4001=ADVANCED_FACE('',(#719),#493,.F.);
#4002=ADVANCED_FACE('',(#720),#494,.F.);
#4003=ADVANCED_FACE('',(#721),#495,.F.);
#4004=ADVANCED_FACE('',(#722),#496,.F.);
#4005=ADVANCED_FACE('',(#723),#497,.F.);
#4006=ADVANCED_FACE('',(#724),#498,.F.);
#4007=ADVANCED_FACE('',(#725),#499,.T.);
#4008=ADVANCED_FACE('',(#726),#209,.T.);
#4009=ADVANCED_FACE('',(#727),#3815,.T.);
#4010=ADVANCED_FACE('',(#728),#210,.T.);
#4011=ADVANCED_FACE('',(#729,#384),#500,.T.);
#4012=ADVANCED_FACE('',(#730),#211,.T.);
#4013=ADVANCED_FACE('',(#731),#3816,.T.);
#4014=ADVANCED_FACE('',(#732),#212,.T.);
#4015=ADVANCED_FACE('',(#733),#501,.T.);
#4016=ADVANCED_FACE('',(#734),#502,.F.);
#4017=ADVANCED_FACE('',(#735),#503,.F.);
#4018=ADVANCED_FACE('',(#736),#504,.F.);
#4019=ADVANCED_FACE('',(#737),#505,.F.);
#4020=ADVANCED_FACE('',(#738),#506,.F.);
#4021=ADVANCED_FACE('',(#739),#507,.F.);
#4022=ADVANCED_FACE('',(#740),#508,.F.);
#4023=ADVANCED_FACE('',(#741),#509,.F.);
#4024=ADVANCED_FACE('',(#742),#510,.F.);
#4025=ADVANCED_FACE('',(#743),#511,.T.);
#4026=ADVANCED_FACE('',(#744),#512,.F.);
#4027=ADVANCED_FACE('',(#745),#513,.F.);
#4028=ADVANCED_FACE('',(#746),#514,.F.);
#4029=ADVANCED_FACE('',(#747,#385),#515,.T.);
#4030=ADVANCED_FACE('',(#748,#386),#516,.F.);
#4031=ADVANCED_FACE('',(#749),#3817,.T.);
#4032=ADVANCED_FACE('',(#750,#387),#3818,.T.);
#4033=ADVANCED_FACE('',(#751),#3819,.T.);
#4034=ADVANCED_FACE('',(#752),#517,.T.);
#4035=ADVANCED_FACE('',(#753),#518,.F.);
#4036=ADVANCED_FACE('',(#754),#3820,.F.);
#4037=ADVANCED_FACE('',(#755),#3821,.T.);
#4038=ADVANCED_FACE('',(#756,#388),#519,.T.);
#4039=ADVANCED_FACE('',(#757,#389),#520,.F.);
#4040=ADVANCED_FACE('',(#758),#521,.T.);
#4041=ADVANCED_FACE('',(#759),#3822,.F.);
#4042=ADVANCED_FACE('',(#760),#522,.T.);
#4043=ADVANCED_FACE('',(#761,#390),#3823,.F.);
#4044=ADVANCED_FACE('',(#762,#391),#3824,.T.);
#4045=ADVANCED_FACE('',(#763,#392),#523,.T.);
#4046=ADVANCED_FACE('',(#764,#393),#524,.F.);
#4047=ADVANCED_FACE('',(#765),#525,.T.);
#4048=ADVANCED_FACE('',(#766),#3825,.F.);
#4049=ADVANCED_FACE('',(#767),#526,.T.);
#4050=ADVANCED_FACE('',(#768),#527,.F.);
#4051=ADVANCED_FACE('',(#769),#528,.F.);
#4052=ADVANCED_FACE('',(#770),#529,.F.);
#4053=ADVANCED_FACE('',(#771,#394),#530,.T.);
#4054=ADVANCED_FACE('',(#772,#395),#3826,.F.);
#4055=ADVANCED_FACE('',(#773),#3827,.F.);
#4056=ADVANCED_FACE('',(#774),#3828,.F.);
#4057=ADVANCED_FACE('',(#775),#3829,.F.);
#4058=ADVANCED_FACE('',(#776),#3830,.F.);
#4059=ADVANCED_FACE('',(#777,#396,#397,#398,#399,#400),#531,.T.);
#4060=ADVANCED_FACE('',(#778),#3831,.T.);
#4061=ADVANCED_FACE('',(#779,#401),#3832,.T.);
#4062=ADVANCED_FACE('',(#780,#402,#403,#404,#405,#406),#532,.F.);
#4063=ADVANCED_FACE('',(#781),#533,.F.);
#4064=ADVANCED_FACE('',(#782),#534,.T.);
#4065=ADVANCED_FACE('',(#783),#535,.T.);
#4066=ADVANCED_FACE('',(#784),#536,.T.);
#4067=ADVANCED_FACE('',(#785),#537,.T.);
#4068=ADVANCED_FACE('',(#786),#538,.T.);
#4069=ADVANCED_FACE('',(#787),#539,.F.);
#4070=ADVANCED_FACE('',(#788),#540,.T.);
#4071=ADVANCED_FACE('',(#789),#541,.T.);
#4072=ADVANCED_FACE('',(#790),#542,.T.);
#4073=ADVANCED_FACE('',(#791),#543,.F.);
#4074=ADVANCED_FACE('',(#792),#544,.F.);
#4075=ADVANCED_FACE('',(#793),#545,.F.);
#4076=ADVANCED_FACE('',(#794),#546,.F.);
#4077=ADVANCED_FACE('',(#795),#547,.F.);
#4078=ADVANCED_FACE('',(#796),#548,.F.);
#4079=ADVANCED_FACE('',(#797),#549,.F.);
#4080=ADVANCED_FACE('',(#798,#407),#550,.T.);
#4081=ADVANCED_FACE('',(#799),#213,.T.);
#4082=ADVANCED_FACE('',(#800),#3833,.T.);
#4083=ADVANCED_FACE('',(#801),#214,.T.);
#4084=ADVANCED_FACE('',(#802),#551,.T.);
#4085=CLOSED_SHELL('',(#3834,#3835,#3836,#3837,#3838,#3839,#3840,#3841,
#3842,#3843));
#4086=CLOSED_SHELL('',(#3844,#3845,#3846,#3847,#3848,#3849,#3850,#3851,
#3852,#3853,#3854,#3855,#3856,#3857,#3858,#3859,#3860,#3861,#3862,#3863,
#3864,#3865,#3866,#3867,#3868,#3869,#3870,#3871,#3872,#3873,#3874,#3875,
#3876,#3877,#3878,#3879,#3880,#3881,#3882,#3883,#3884,#3885));
#4087=CLOSED_SHELL('',(#3886,#3887,#3888,#3889));
#4088=CLOSED_SHELL('',(#3890,#3891,#3892,#3893,#3894,#3895,#3896,#3897,
#3898,#3899,#3900,#3901));
#4089=CLOSED_SHELL('',(#3902,#3903,#3904,#3905));
#4090=CLOSED_SHELL('',(#3906,#3907,#3908,#3909,#3910,#3911,#3912,#3913,
#3914,#3915,#3916,#3917,#3918,#3919,#3920,#3921,#3922,#3923,#3924,#3925,
#3926));
#4091=CLOSED_SHELL('',(#3927,#3928,#3929,#3930,#3931,#3932));
#4092=CLOSED_SHELL('',(#3933,#3934,#3935,#3936,#3937,#3938));
#4093=CLOSED_SHELL('',(#3939,#3940,#3941,#3942,#3943,#3944,#3945,#3946));
#4094=CLOSED_SHELL('',(#3947,#3948,#3949,#3950,#3951,#3952,#3953,#3954));
#4095=CLOSED_SHELL('',(#3955));
#4096=CLOSED_SHELL('',(#3956));
#4097=CLOSED_SHELL('',(#3957));
#4098=CLOSED_SHELL('',(#3958));
#4099=CLOSED_SHELL('',(#3959));
#4100=CLOSED_SHELL('',(#3960));
#4101=CLOSED_SHELL('',(#3961));
#4102=CLOSED_SHELL('',(#3962));
#4103=CLOSED_SHELL('',(#3963,#3964,#3965,#3966,#3967,#3968,#3969,#3970,
#3971,#3972,#3973,#3974,#3975,#3976,#3977,#3978,#3979,#3980,#3981));
#4104=CLOSED_SHELL('',(#3982,#3983,#3984,#3985));
#4105=CLOSED_SHELL('',(#3986,#3987,#3988,#3989));
#4106=CLOSED_SHELL('',(#3990,#3991,#3992,#3993,#3994,#3995,#3996,#3997,
#3998));
#4107=CLOSED_SHELL('',(#3999,#4000,#4001,#4002,#4003,#4004,#4005,#4006));
#4108=CLOSED_SHELL('',(#4007,#4008,#4009,#4010,#4011,#4012,#4013,#4014,
#4015));
#4109=CLOSED_SHELL('',(#4016,#4017,#4018,#4019,#4020,#4021,#4022,#4023));
#4110=CLOSED_SHELL('',(#4024,#4025,#4026,#4027,#4028,#4029,#4030,#4031,
#4032,#4033,#4034,#4035));
#4111=CLOSED_SHELL('',(#4036,#4037,#4038,#4039));
#4112=CLOSED_SHELL('',(#4040,#4041,#4042,#4043,#4044,#4045,#4046));
#4113=CLOSED_SHELL('',(#4047,#4048,#4049,#4050,#4051,#4052,#4053,#4054,
#4055,#4056,#4057,#4058,#4059,#4060,#4061,#4062));
#4114=CLOSED_SHELL('',(#4063,#4064,#4065,#4066,#4067,#4068,#4069,#4070,
#4071,#4072));
#4115=CLOSED_SHELL('',(#4073,#4074,#4075,#4076,#4077,#4078,#4079,#4080,
#4081,#4082,#4083,#4084));
#4116=DERIVED_UNIT_ELEMENT(#4158,1.);
#4117=DERIVED_UNIT_ELEMENT(#7873,-3.);
#4118=DERIVED_UNIT_ELEMENT(#4158,1.);
#4119=DERIVED_UNIT_ELEMENT(#7873,-3.);
#4120=DERIVED_UNIT_ELEMENT(#4158,1.);
#4121=DERIVED_UNIT_ELEMENT(#7873,-3.);
#4122=DERIVED_UNIT_ELEMENT(#4158,1.);
#4123=DERIVED_UNIT_ELEMENT(#7873,-3.);
#4124=DERIVED_UNIT_ELEMENT(#4158,1.);
#4125=DERIVED_UNIT_ELEMENT(#7873,-3.);
#4126=DERIVED_UNIT_ELEMENT(#4158,1.);
#4127=DERIVED_UNIT_ELEMENT(#7873,-3.);
#4128=DERIVED_UNIT_ELEMENT(#4158,1.);
#4129=DERIVED_UNIT_ELEMENT(#7873,-3.);
#4130=DERIVED_UNIT_ELEMENT(#4158,1.);
#4131=DERIVED_UNIT_ELEMENT(#7873,-3.);
#4132=DERIVED_UNIT_ELEMENT(#4158,1.);
#4133=DERIVED_UNIT_ELEMENT(#7873,-3.);
#4134=DERIVED_UNIT_ELEMENT(#4158,1.);
#4135=DERIVED_UNIT_ELEMENT(#7873,-3.);
#4136=DERIVED_UNIT_ELEMENT(#4158,1.);
#4137=DERIVED_UNIT_ELEMENT(#7873,-3.);
#4138=DERIVED_UNIT_ELEMENT(#4158,1.);
#4139=DERIVED_UNIT_ELEMENT(#7873,-3.);
#4140=DERIVED_UNIT_ELEMENT(#4158,1.);
#4141=DERIVED_UNIT_ELEMENT(#7873,-3.);
#4142=DERIVED_UNIT_ELEMENT(#4158,1.);
#4143=DERIVED_UNIT_ELEMENT(#7873,-3.);
#4144=DERIVED_UNIT_ELEMENT(#4158,1.);
#4145=DERIVED_UNIT_ELEMENT(#7873,-3.);
#4146=DERIVED_UNIT_ELEMENT(#4158,1.);
#4147=DERIVED_UNIT_ELEMENT(#7873,-3.);
#4148=DERIVED_UNIT_ELEMENT(#4158,1.);
#4149=DERIVED_UNIT_ELEMENT(#7873,-3.);
#4150=DERIVED_UNIT_ELEMENT(#4158,1.);
#4151=DERIVED_UNIT_ELEMENT(#7873,-3.);
#4152=DERIVED_UNIT_ELEMENT(#4158,1.);
#4153=DERIVED_UNIT_ELEMENT(#7873,-3.);
#4154=DERIVED_UNIT_ELEMENT(#4158,1.);
#4155=DERIVED_UNIT_ELEMENT(#7873,-3.);
#4156=DERIVED_UNIT_ELEMENT(#4158,1.);
#4157=DERIVED_UNIT_ELEMENT(#7873,-3.);
#4158=(
MASS_UNIT()
NAMED_UNIT(*)
SI_UNIT(.KILO.,.GRAM.)
);
#4159=DERIVED_UNIT((#4116,#4117));
#4160=DERIVED_UNIT((#4118,#4119));
#4161=DERIVED_UNIT((#4120,#4121));
#4162=DERIVED_UNIT((#4122,#4123));
#4163=DERIVED_UNIT((#4124,#4125));
#4164=DERIVED_UNIT((#4126,#4127));
#4165=DERIVED_UNIT((#4128,#4129));
#4166=DERIVED_UNIT((#4130,#4131));
#4167=DERIVED_UNIT((#4132,#4133));
#4168=DERIVED_UNIT((#4134,#4135));
#4169=DERIVED_UNIT((#4136,#4137));
#4170=DERIVED_UNIT((#4138,#4139));
#4171=DERIVED_UNIT((#4140,#4141));
#4172=DERIVED_UNIT((#4142,#4143));
#4173=DERIVED_UNIT((#4144,#4145));
#4174=DERIVED_UNIT((#4146,#4147));
#4175=DERIVED_UNIT((#4148,#4149));
#4176=DERIVED_UNIT((#4150,#4151));
#4177=DERIVED_UNIT((#4152,#4153));
#4178=DERIVED_UNIT((#4154,#4155));
#4179=DERIVED_UNIT((#4156,#4157));
#4180=MEASURE_REPRESENTATION_ITEM('density measure',
POSITIVE_RATIO_MEASURE(7850.),#4159);
#4181=MEASURE_REPRESENTATION_ITEM('density measure',
POSITIVE_RATIO_MEASURE(7850.),#4160);
#4182=MEASURE_REPRESENTATION_ITEM('density measure',
POSITIVE_RATIO_MEASURE(7850.),#4161);
#4183=MEASURE_REPRESENTATION_ITEM('density measure',
POSITIVE_RATIO_MEASURE(7850.),#4162);
#4184=MEASURE_REPRESENTATION_ITEM('density measure',
POSITIVE_RATIO_MEASURE(7850.),#4163);
#4185=MEASURE_REPRESENTATION_ITEM('density measure',
POSITIVE_RATIO_MEASURE(7850.),#4164);
#4186=MEASURE_REPRESENTATION_ITEM('density measure',
POSITIVE_RATIO_MEASURE(7850.),#4165);
#4187=MEASURE_REPRESENTATION_ITEM('density measure',
POSITIVE_RATIO_MEASURE(7850.),#4166);
#4188=MEASURE_REPRESENTATION_ITEM('density measure',
POSITIVE_RATIO_MEASURE(7850.),#4167);
#4189=MEASURE_REPRESENTATION_ITEM('density measure',
POSITIVE_RATIO_MEASURE(7850.),#4168);
#4190=MEASURE_REPRESENTATION_ITEM('density measure',
POSITIVE_RATIO_MEASURE(7850.),#4169);
#4191=MEASURE_REPRESENTATION_ITEM('density measure',
POSITIVE_RATIO_MEASURE(7850.),#4170);
#4192=MEASURE_REPRESENTATION_ITEM('density measure',
POSITIVE_RATIO_MEASURE(7850.),#4171);
#4193=MEASURE_REPRESENTATION_ITEM('density measure',
POSITIVE_RATIO_MEASURE(7850.),#4172);
#4194=MEASURE_REPRESENTATION_ITEM('density measure',
POSITIVE_RATIO_MEASURE(7850.),#4173);
#4195=MEASURE_REPRESENTATION_ITEM('density measure',
POSITIVE_RATIO_MEASURE(7850.),#4174);
#4196=MEASURE_REPRESENTATION_ITEM('density measure',
POSITIVE_RATIO_MEASURE(7850.),#4175);
#4197=MEASURE_REPRESENTATION_ITEM('density measure',
POSITIVE_RATIO_MEASURE(7850.),#4176);
#4198=MEASURE_REPRESENTATION_ITEM('density measure',
POSITIVE_RATIO_MEASURE(7850.),#4177);
#4199=MEASURE_REPRESENTATION_ITEM('density measure',
POSITIVE_RATIO_MEASURE(7850.),#4178);
#4200=MEASURE_REPRESENTATION_ITEM('density measure',
POSITIVE_RATIO_MEASURE(7850.),#4179);
#4201=PROPERTY_DEFINITION_REPRESENTATION(#4306,#4243);
#4202=PROPERTY_DEFINITION_REPRESENTATION(#4307,#4244);
#4203=PROPERTY_DEFINITION_REPRESENTATION(#4308,#4245);
#4204=PROPERTY_DEFINITION_REPRESENTATION(#4309,#4246);
#4205=PROPERTY_DEFINITION_REPRESENTATION(#4310,#4247);
#4206=PROPERTY_DEFINITION_REPRESENTATION(#4311,#4248);
#4207=PROPERTY_DEFINITION_REPRESENTATION(#4312,#4249);
#4208=PROPERTY_DEFINITION_REPRESENTATION(#4313,#4250);
#4209=PROPERTY_DEFINITION_REPRESENTATION(#4314,#4251);
#4210=PROPERTY_DEFINITION_REPRESENTATION(#4315,#4252);
#4211=PROPERTY_DEFINITION_REPRESENTATION(#4316,#4253);
#4212=PROPERTY_DEFINITION_REPRESENTATION(#4317,#4254);
#4213=PROPERTY_DEFINITION_REPRESENTATION(#4318,#4255);
#4214=PROPERTY_DEFINITION_REPRESENTATION(#4319,#4256);
#4215=PROPERTY_DEFINITION_REPRESENTATION(#4320,#4257);
#4216=PROPERTY_DEFINITION_REPRESENTATION(#4321,#4258);
#4217=PROPERTY_DEFINITION_REPRESENTATION(#4322,#4259);
#4218=PROPERTY_DEFINITION_REPRESENTATION(#4323,#4260);
#4219=PROPERTY_DEFINITION_REPRESENTATION(#4324,#4261);
#4220=PROPERTY_DEFINITION_REPRESENTATION(#4325,#4262);
#4221=PROPERTY_DEFINITION_REPRESENTATION(#4326,#4263);
#4222=PROPERTY_DEFINITION_REPRESENTATION(#4327,#4264);
#4223=PROPERTY_DEFINITION_REPRESENTATION(#4328,#4265);
#4224=PROPERTY_DEFINITION_REPRESENTATION(#4329,#4266);
#4225=PROPERTY_DEFINITION_REPRESENTATION(#4330,#4267);
#4226=PROPERTY_DEFINITION_REPRESENTATION(#4331,#4268);
#4227=PROPERTY_DEFINITION_REPRESENTATION(#4332,#4269);
#4228=PROPERTY_DEFINITION_REPRESENTATION(#4333,#4270);
#4229=PROPERTY_DEFINITION_REPRESENTATION(#4334,#4271);
#4230=PROPERTY_DEFINITION_REPRESENTATION(#4335,#4272);
#4231=PROPERTY_DEFINITION_REPRESENTATION(#4336,#4273);
#4232=PROPERTY_DEFINITION_REPRESENTATION(#4337,#4274);
#4233=PROPERTY_DEFINITION_REPRESENTATION(#4338,#4275);
#4234=PROPERTY_DEFINITION_REPRESENTATION(#4339,#4276);
#4235=PROPERTY_DEFINITION_REPRESENTATION(#4340,#4277);
#4236=PROPERTY_DEFINITION_REPRESENTATION(#4341,#4278);
#4237=PROPERTY_DEFINITION_REPRESENTATION(#4342,#4279);
#4238=PROPERTY_DEFINITION_REPRESENTATION(#4343,#4280);
#4239=PROPERTY_DEFINITION_REPRESENTATION(#4344,#4281);
#4240=PROPERTY_DEFINITION_REPRESENTATION(#4345,#4282);
#4241=PROPERTY_DEFINITION_REPRESENTATION(#4346,#4283);
#4242=PROPERTY_DEFINITION_REPRESENTATION(#4347,#4284);
#4243=REPRESENTATION('material name',(#4285),#7848);
#4244=REPRESENTATION('density',(#4180),#7848);
#4245=REPRESENTATION('material name',(#4286),#7849);
#4246=REPRESENTATION('density',(#4181),#7849);
#4247=REPRESENTATION('material name',(#4287),#7850);
#4248=REPRESENTATION('density',(#4182),#7850);
#4249=REPRESENTATION('material name',(#4288),#7851);
#4250=REPRESENTATION('density',(#4183),#7851);
#4251=REPRESENTATION('material name',(#4289),#7852);
#4252=REPRESENTATION('density',(#4184),#7852);
#4253=REPRESENTATION('material name',(#4290),#7853);
#4254=REPRESENTATION('density',(#4185),#7853);
#4255=REPRESENTATION('material name',(#4291),#7854);
#4256=REPRESENTATION('density',(#4186),#7854);
#4257=REPRESENTATION('material name',(#4292),#7855);
#4258=REPRESENTATION('density',(#4187),#7855);
#4259=REPRESENTATION('material name',(#4293),#7857);
#4260=REPRESENTATION('density',(#4188),#7857);
#4261=REPRESENTATION('material name',(#4294),#7858);
#4262=REPRESENTATION('density',(#4189),#7858);
#4263=REPRESENTATION('material name',(#4295),#7859);
#4264=REPRESENTATION('density',(#4190),#7859);
#4265=REPRESENTATION('material name',(#4296),#7860);
#4266=REPRESENTATION('density',(#4191),#7860);
#4267=REPRESENTATION('material name',(#4297),#7861);
#4268=REPRESENTATION('density',(#4192),#7861);
#4269=REPRESENTATION('material name',(#4298),#7862);
#4270=REPRESENTATION('density',(#4193),#7862);
#4271=REPRESENTATION('material name',(#4299),#7863);
#4272=REPRESENTATION('density',(#4194),#7863);
#4273=REPRESENTATION('material name',(#4300),#7865);
#4274=REPRESENTATION('density',(#4195),#7865);
#4275=REPRESENTATION('material name',(#4301),#7866);
#4276=REPRESENTATION('density',(#4196),#7866);
#4277=REPRESENTATION('material name',(#4302),#7867);
#4278=REPRESENTATION('density',(#4197),#7867);
#4279=REPRESENTATION('material name',(#4303),#7868);
#4280=REPRESENTATION('density',(#4198),#7868);
#4281=REPRESENTATION('material name',(#4304),#7869);
#4282=REPRESENTATION('density',(#4199),#7869);
#4283=REPRESENTATION('material name',(#4305),#7870);
#4284=REPRESENTATION('density',(#4200),#7870);
#4285=DESCRIPTIVE_REPRESENTATION_ITEM('Steel','Steel');
#4286=DESCRIPTIVE_REPRESENTATION_ITEM('Steel','Steel');
#4287=DESCRIPTIVE_REPRESENTATION_ITEM('Steel','Steel');
#4288=DESCRIPTIVE_REPRESENTATION_ITEM('Steel','Steel');
#4289=DESCRIPTIVE_REPRESENTATION_ITEM('Steel','Steel');
#4290=DESCRIPTIVE_REPRESENTATION_ITEM('Steel','Steel');
#4291=DESCRIPTIVE_REPRESENTATION_ITEM('Steel','Steel');
#4292=DESCRIPTIVE_REPRESENTATION_ITEM('Steel','Steel');
#4293=DESCRIPTIVE_REPRESENTATION_ITEM('Steel','Steel');
#4294=DESCRIPTIVE_REPRESENTATION_ITEM('Steel','Steel');
#4295=DESCRIPTIVE_REPRESENTATION_ITEM('Steel','Steel');
#4296=DESCRIPTIVE_REPRESENTATION_ITEM('Steel','Steel');
#4297=DESCRIPTIVE_REPRESENTATION_ITEM('Steel','Steel');
#4298=DESCRIPTIVE_REPRESENTATION_ITEM('Steel','Steel');
#4299=DESCRIPTIVE_REPRESENTATION_ITEM('Steel','Steel');
#4300=DESCRIPTIVE_REPRESENTATION_ITEM('Steel','Steel');
#4301=DESCRIPTIVE_REPRESENTATION_ITEM('Steel','Steel');
#4302=DESCRIPTIVE_REPRESENTATION_ITEM('Steel','Steel');
#4303=DESCRIPTIVE_REPRESENTATION_ITEM('Steel','Steel');
#4304=DESCRIPTIVE_REPRESENTATION_ITEM('Steel','Steel');
#4305=DESCRIPTIVE_REPRESENTATION_ITEM('Steel','Steel');
#4306=PROPERTY_DEFINITION('material property','material name',#7990);
#4307=PROPERTY_DEFINITION('material property','density of part',#7990);
#4308=PROPERTY_DEFINITION('material property','material name',#7991);
#4309=PROPERTY_DEFINITION('material property','density of part',#7991);
#4310=PROPERTY_DEFINITION('material property','material name',#7992);
#4311=PROPERTY_DEFINITION('material property','density of part',#7992);
#4312=PROPERTY_DEFINITION('material property','material name',#7993);
#4313=PROPERTY_DEFINITION('material property','density of part',#7993);
#4314=PROPERTY_DEFINITION('material property','material name',#7994);
#4315=PROPERTY_DEFINITION('material property','density of part',#7994);
#4316=PROPERTY_DEFINITION('material property','material name',#7995);
#4317=PROPERTY_DEFINITION('material property','density of part',#7995);
#4318=PROPERTY_DEFINITION('material property','material name',#7996);
#4319=PROPERTY_DEFINITION('material property','density of part',#7996);
#4320=PROPERTY_DEFINITION('material property','material name',#7997);
#4321=PROPERTY_DEFINITION('material property','density of part',#7997);
#4322=PROPERTY_DEFINITION('material property','material name',#7999);
#4323=PROPERTY_DEFINITION('material property','density of part',#7999);
#4324=PROPERTY_DEFINITION('material property','material name',#8000);
#4325=PROPERTY_DEFINITION('material property','density of part',#8000);
#4326=PROPERTY_DEFINITION('material property','material name',#8001);
#4327=PROPERTY_DEFINITION('material property','density of part',#8001);
#4328=PROPERTY_DEFINITION('material property','material name',#8002);
#4329=PROPERTY_DEFINITION('material property','density of part',#8002);
#4330=PROPERTY_DEFINITION('material property','material name',#8003);
#4331=PROPERTY_DEFINITION('material property','density of part',#8003);
#4332=PROPERTY_DEFINITION('material property','material name',#8004);
#4333=PROPERTY_DEFINITION('material property','density of part',#8004);
#4334=PROPERTY_DEFINITION('material property','material name',#8005);
#4335=PROPERTY_DEFINITION('material property','density of part',#8005);
#4336=PROPERTY_DEFINITION('material property','material name',#8007);
#4337=PROPERTY_DEFINITION('material property','density of part',#8007);
#4338=PROPERTY_DEFINITION('material property','material name',#8008);
#4339=PROPERTY_DEFINITION('material property','density of part',#8008);
#4340=PROPERTY_DEFINITION('material property','material name',#8009);
#4341=PROPERTY_DEFINITION('material property','density of part',#8009);
#4342=PROPERTY_DEFINITION('material property','material name',#8010);
#4343=PROPERTY_DEFINITION('material property','density of part',#8010);
#4344=PROPERTY_DEFINITION('material property','material name',#8011);
#4345=PROPERTY_DEFINITION('material property','density of part',#8011);
#4346=PROPERTY_DEFINITION('material property','material name',#8012);
#4347=PROPERTY_DEFINITION('material property','density of part',#8012);
#4348=AXIS2_PLACEMENT_3D('',#6206,#4880,#4881);
#4349=AXIS2_PLACEMENT_3D('',#6207,#4882,#4883);
#4350=AXIS2_PLACEMENT_3D('',#6208,#4884,#4885);
#4351=AXIS2_PLACEMENT_3D('',#6209,#4886,#4887);
#4352=AXIS2_PLACEMENT_3D('',#6211,#4888,#4889);
#4353=AXIS2_PLACEMENT_3D('',#6214,#4891,#4892);
#4354=AXIS2_PLACEMENT_3D('',#6215,#4893,#4894);
#4355=AXIS2_PLACEMENT_3D('',#6217,#4895,#4896);
#4356=AXIS2_PLACEMENT_3D('',#6220,#4898,#4899);
#4357=AXIS2_PLACEMENT_3D('',#6221,#4900,#4901);
#4358=AXIS2_PLACEMENT_3D('',#6223,#4902,#4903);
#4359=AXIS2_PLACEMENT_3D('',#6226,#4905,#4906);
#4360=AXIS2_PLACEMENT_3D('',#6227,#4907,#4908);
#4361=AXIS2_PLACEMENT_3D('',#6229,#4909,#4910);
#4362=AXIS2_PLACEMENT_3D('',#6232,#4912,#4913);
#4363=AXIS2_PLACEMENT_3D('',#6233,#4914,#4915);
#4364=AXIS2_PLACEMENT_3D('',#6242,#4920,#4921);
#4365=AXIS2_PLACEMENT_3D('',#6248,#4925,#4926);
#4366=AXIS2_PLACEMENT_3D('',#6254,#4930,#4931);
#4367=AXIS2_PLACEMENT_3D('',#6257,#4934,#4935);
#4368=AXIS2_PLACEMENT_3D('',#6258,#4936,#4937);
#4369=AXIS2_PLACEMENT_3D('',#6259,#4938,#4939);
#4370=AXIS2_PLACEMENT_3D('',#6260,#4940,#4941);
#4371=AXIS2_PLACEMENT_3D('',#6262,#4942,#4943);
#4372=AXIS2_PLACEMENT_3D('',#6265,#4945,#4946);
#4373=AXIS2_PLACEMENT_3D('',#6266,#4947,#4948);
#4374=AXIS2_PLACEMENT_3D('',#6267,#4949,#4950);
#4375=AXIS2_PLACEMENT_3D('',#6269,#4951,#4952);
#4376=AXIS2_PLACEMENT_3D('',#6272,#4954,#4955);
#4377=AXIS2_PLACEMENT_3D('',#6273,#4956,#4957);
#4378=AXIS2_PLACEMENT_3D('',#6274,#4958,#4959);
#4379=AXIS2_PLACEMENT_3D('',#6276,#4960,#4961);
#4380=AXIS2_PLACEMENT_3D('',#6279,#4963,#4964);
#4381=AXIS2_PLACEMENT_3D('',#6280,#4965,#4966);
#4382=AXIS2_PLACEMENT_3D('',#6281,#4967,#4968);
#4383=AXIS2_PLACEMENT_3D('',#6283,#4969,#4970);
#4384=AXIS2_PLACEMENT_3D('',#6286,#4972,#4973);
#4385=AXIS2_PLACEMENT_3D('',#6287,#4974,#4975);
#4386=AXIS2_PLACEMENT_3D('',#6288,#4976,#4977);
#4387=AXIS2_PLACEMENT_3D('',#6290,#4978,#4979);
#4388=AXIS2_PLACEMENT_3D('',#6293,#4981,#4982);
#4389=AXIS2_PLACEMENT_3D('',#6294,#4983,#4984);
#4390=AXIS2_PLACEMENT_3D('',#6295,#4985,#4986);
#4391=AXIS2_PLACEMENT_3D('',#6297,#4987,#4988);
#4392=AXIS2_PLACEMENT_3D('',#6300,#4990,#4991);
#4393=AXIS2_PLACEMENT_3D('',#6301,#4992,#4993);
#4394=AXIS2_PLACEMENT_3D('',#6302,#4994,#4995);
#4395=AXIS2_PLACEMENT_3D('',#6304,#4996,#4997);
#4396=AXIS2_PLACEMENT_3D('',#6307,#4999,#5000);
#4397=AXIS2_PLACEMENT_3D('',#6308,#5001,#5002);
#4398=AXIS2_PLACEMENT_3D('',#6309,#5003,#5004);
#4399=AXIS2_PLACEMENT_3D('',#6311,#5005,#5006);
#4400=AXIS2_PLACEMENT_3D('',#6314,#5008,#5009);
#4401=AXIS2_PLACEMENT_3D('',#6315,#5010,#5011);
#4402=AXIS2_PLACEMENT_3D('',#6316,#5012,#5013);
#4403=AXIS2_PLACEMENT_3D('',#6318,#5014,#5015);
#4404=AXIS2_PLACEMENT_3D('',#6321,#5017,#5018);
#4405=AXIS2_PLACEMENT_3D('',#6322,#5019,#5020);
#4406=AXIS2_PLACEMENT_3D('',#6324,#5021,#5022);
#4407=AXIS2_PLACEMENT_3D('',#6327,#5024,#5025);
#4408=AXIS2_PLACEMENT_3D('',#6328,#5026,#5027);
#4409=AXIS2_PLACEMENT_3D('',#6330,#5028,#5029);
#4410=AXIS2_PLACEMENT_3D('',#6333,#5031,#5032);
#4411=AXIS2_PLACEMENT_3D('',#6334,#5033,#5034);
#4412=AXIS2_PLACEMENT_3D('',#6336,#5035,#5036);
#4413=AXIS2_PLACEMENT_3D('',#6339,#5038,#5039);
#4414=AXIS2_PLACEMENT_3D('',#6340,#5040,#5041);
#4415=AXIS2_PLACEMENT_3D('',#6343,#5042,#5043);
#4416=AXIS2_PLACEMENT_3D('',#6349,#5047,#5048);
#4417=AXIS2_PLACEMENT_3D('',#6351,#5049,#5050);
#4418=AXIS2_PLACEMENT_3D('',#6357,#5054,#5055);
#4419=AXIS2_PLACEMENT_3D('',#6360,#5056,#5057);
#4420=AXIS2_PLACEMENT_3D('',#6366,#5061,#5062);
#4421=AXIS2_PLACEMENT_3D('',#6368,#5063,#5064);
#4422=AXIS2_PLACEMENT_3D('',#6374,#5068,#5069);
#4423=AXIS2_PLACEMENT_3D('',#6377,#5072,#5073);
#4424=AXIS2_PLACEMENT_3D('',#6380,#5076,#5077);
#4425=AXIS2_PLACEMENT_3D('',#6382,#5079,#5080);
#4426=AXIS2_PLACEMENT_3D('',#6384,#5082,#5083);
#4427=AXIS2_PLACEMENT_3D('',#6385,#5084,#5085);
#4428=AXIS2_PLACEMENT_3D('',#6388,#5086,#5087);
#4429=AXIS2_PLACEMENT_3D('',#6394,#5091,#5092);
#4430=AXIS2_PLACEMENT_3D('',#6396,#5093,#5094);
#4431=AXIS2_PLACEMENT_3D('',#6402,#5098,#5099);
#4432=AXIS2_PLACEMENT_3D('',#6405,#5100,#5101);
#4433=AXIS2_PLACEMENT_3D('',#6411,#5105,#5106);
#4434=AXIS2_PLACEMENT_3D('',#6413,#5107,#5108);
#4435=AXIS2_PLACEMENT_3D('',#6419,#5112,#5113);
#4436=AXIS2_PLACEMENT_3D('',#6422,#5116,#5117);
#4437=AXIS2_PLACEMENT_3D('',#6425,#5120,#5121);
#4438=AXIS2_PLACEMENT_3D('',#6427,#5123,#5124);
#4439=AXIS2_PLACEMENT_3D('',#6429,#5126,#5127);
#4440=AXIS2_PLACEMENT_3D('',#6430,#5128,#5129);
#4441=AXIS2_PLACEMENT_3D('',#6432,#5130,#5131);
#4442=AXIS2_PLACEMENT_3D('',#6435,#5133,#5134);
#4443=AXIS2_PLACEMENT_3D('',#6436,#5135,#5136);
#4444=AXIS2_PLACEMENT_3D('',#6438,#5137,#5138);
#4445=AXIS2_PLACEMENT_3D('',#6441,#5140,#5141);
#4446=AXIS2_PLACEMENT_3D('',#6442,#5142,#5143);
#4447=AXIS2_PLACEMENT_3D('',#6443,#5144,#5145);
#4448=AXIS2_PLACEMENT_3D('',#6444,#5146,#5147);
#4449=AXIS2_PLACEMENT_3D('',#6445,#5148,#5149);
#4450=AXIS2_PLACEMENT_3D('',#6447,#5150,#5151);
#4451=AXIS2_PLACEMENT_3D('',#6450,#5153,#5154);
#4452=AXIS2_PLACEMENT_3D('',#6451,#5155,#5156);
#4453=AXIS2_PLACEMENT_3D('',#6453,#5157,#5158);
#4454=AXIS2_PLACEMENT_3D('',#6456,#5160,#5161);
#4455=AXIS2_PLACEMENT_3D('',#6457,#5162,#5163);
#4456=AXIS2_PLACEMENT_3D('',#6458,#5164,#5165);
#4457=AXIS2_PLACEMENT_3D('',#6459,#5166,#5167);
#4458=AXIS2_PLACEMENT_3D('',#6460,#5168,#5169);
#4459=AXIS2_PLACEMENT_3D('',#6462,#5170,#5171);
#4460=AXIS2_PLACEMENT_3D('',#6465,#5173,#5174);
#4461=AXIS2_PLACEMENT_3D('',#6466,#5175,#5176);
#4462=AXIS2_PLACEMENT_3D('',#6468,#5177,#5178);
#4463=AXIS2_PLACEMENT_3D('',#6471,#5180,#5181);
#4464=AXIS2_PLACEMENT_3D('',#6472,#5182,#5183);
#4465=AXIS2_PLACEMENT_3D('',#6474,#5184,#5185);
#4466=AXIS2_PLACEMENT_3D('',#6477,#5187,#5188);
#4467=AXIS2_PLACEMENT_3D('',#6478,#5189,#5190);
#4468=AXIS2_PLACEMENT_3D('',#6480,#5191,#5192);
#4469=AXIS2_PLACEMENT_3D('',#6483,#5194,#5195);
#4470=AXIS2_PLACEMENT_3D('',#6484,#5196,#5197);
#4471=AXIS2_PLACEMENT_3D('',#6486,#5198,#5199);
#4472=AXIS2_PLACEMENT_3D('',#6489,#5201,#5202);
#4473=AXIS2_PLACEMENT_3D('',#6490,#5203,#5204);
#4474=AXIS2_PLACEMENT_3D('',#6492,#5205,#5206);
#4475=AXIS2_PLACEMENT_3D('',#6493,#5207,#5208);
#4476=AXIS2_PLACEMENT_3D('',#6495,#5209,#5210);
#4477=AXIS2_PLACEMENT_3D('',#6498,#5212,#5213);
#4478=AXIS2_PLACEMENT_3D('',#6499,#5214,#5215);
#4479=AXIS2_PLACEMENT_3D('',#6501,#5216,#5217);
#4480=AXIS2_PLACEMENT_3D('',#6502,#5218,#5219);
#4481=AXIS2_PLACEMENT_3D('',#6504,#5221,#5222);
#4482=AXIS2_PLACEMENT_3D('',#6506,#5223,#5224);
#4483=AXIS2_PLACEMENT_3D('',#6509,#5226,#5227);
#4484=AXIS2_PLACEMENT_3D('',#6510,#5228,#5229);
#4485=AXIS2_PLACEMENT_3D('',#6511,#5230,#5231);
#4486=AXIS2_PLACEMENT_3D('',#6512,#5232,#5233);
#4487=AXIS2_PLACEMENT_3D('',#6513,#5234,#5235);
#4488=AXIS2_PLACEMENT_3D('',#6515,#5236,#5237);
#4489=AXIS2_PLACEMENT_3D('',#6518,#5239,#5240);
#4490=AXIS2_PLACEMENT_3D('',#6519,#5241,#5242);
#4491=AXIS2_PLACEMENT_3D('',#6521,#5243,#5244);
#4492=AXIS2_PLACEMENT_3D('',#6524,#5246,#5247);
#4493=AXIS2_PLACEMENT_3D('',#6525,#5248,#5249);
#4494=AXIS2_PLACEMENT_3D('',#6526,#5250,#5251);
#4495=AXIS2_PLACEMENT_3D('',#6527,#5252,#5253);
#4496=AXIS2_PLACEMENT_3D('',#6528,#5254,#5255);
#4497=AXIS2_PLACEMENT_3D('',#6530,#5256,#5257);
#4498=AXIS2_PLACEMENT_3D('',#6533,#5259,#5260);
#4499=AXIS2_PLACEMENT_3D('',#6534,#5261,#5262);
#4500=AXIS2_PLACEMENT_3D('',#6536,#5263,#5264);
#4501=AXIS2_PLACEMENT_3D('',#6537,#5265,#5266);
#4502=AXIS2_PLACEMENT_3D('',#6539,#5267,#5268);
#4503=AXIS2_PLACEMENT_3D('',#6542,#5270,#5271);
#4504=AXIS2_PLACEMENT_3D('',#6543,#5272,#5273);
#4505=AXIS2_PLACEMENT_3D('',#6545,#5274,#5275);
#4506=AXIS2_PLACEMENT_3D('',#6546,#5276,#5277);
#4507=AXIS2_PLACEMENT_3D('',#6548,#5278,#5279);
#4508=AXIS2_PLACEMENT_3D('',#6551,#5281,#5282);
#4509=AXIS2_PLACEMENT_3D('',#6552,#5283,#5284);
#4510=AXIS2_PLACEMENT_3D('',#6554,#5285,#5286);
#4511=AXIS2_PLACEMENT_3D('',#6555,#5287,#5288);
#4512=AXIS2_PLACEMENT_3D('',#6557,#5289,#5290);
#4513=AXIS2_PLACEMENT_3D('',#6560,#5292,#5293);
#4514=AXIS2_PLACEMENT_3D('',#6561,#5294,#5295);
#4515=AXIS2_PLACEMENT_3D('',#6563,#5296,#5297);
#4516=AXIS2_PLACEMENT_3D('',#6564,#5298,#5299);
#4517=AXIS2_PLACEMENT_3D('',#6566,#5300,#5301);
#4518=AXIS2_PLACEMENT_3D('',#6568,#5303,#5304);
#4519=AXIS2_PLACEMENT_3D('',#6570,#5305,#5306);
#4520=AXIS2_PLACEMENT_3D('',#6572,#5308,#5309);
#4521=AXIS2_PLACEMENT_3D('',#6574,#5310,#5311);
#4522=AXIS2_PLACEMENT_3D('',#6576,#5313,#5314);
#4523=AXIS2_PLACEMENT_3D('',#6578,#5315,#5316);
#4524=AXIS2_PLACEMENT_3D('',#6580,#5318,#5319);
#4525=AXIS2_PLACEMENT_3D('',#6582,#5320,#5321);
#4526=AXIS2_PLACEMENT_3D('',#6584,#5322,#5323);
#4527=AXIS2_PLACEMENT_3D('',#6585,#5324,#5325);
#4528=AXIS2_PLACEMENT_3D('',#6588,#5327,#5328);
#4529=AXIS2_PLACEMENT_3D('',#6589,#5329,#5330);
#4530=AXIS2_PLACEMENT_3D('',#6591,#5331,#5332);
#4531=AXIS2_PLACEMENT_3D('',#6594,#5334,#5335);
#4532=AXIS2_PLACEMENT_3D('',#6595,#5336,#5337);
#4533=AXIS2_PLACEMENT_3D('',#6596,#5338,#5339);
#4534=AXIS2_PLACEMENT_3D('',#6599,#5341,#5342);
#4535=AXIS2_PLACEMENT_3D('',#6600,#5343,#5344);
#4536=AXIS2_PLACEMENT_3D('',#6601,#5345,#5346);
#4537=AXIS2_PLACEMENT_3D('',#6603,#5347,#5348);
#4538=AXIS2_PLACEMENT_3D('',#6606,#5350,#5351);
#4539=AXIS2_PLACEMENT_3D('',#6607,#5352,#5353);
#4540=AXIS2_PLACEMENT_3D('',#6608,#5354,#5355);
#4541=AXIS2_PLACEMENT_3D('',#6609,#5356,#5357);
#4542=AXIS2_PLACEMENT_3D('',#6610,#5358,#5359);
#4543=AXIS2_PLACEMENT_3D('',#6619,#5364,#5365);
#4544=AXIS2_PLACEMENT_3D('',#6625,#5369,#5370);
#4545=AXIS2_PLACEMENT_3D('',#6631,#5374,#5375);
#4546=AXIS2_PLACEMENT_3D('',#6634,#5378,#5379);
#4547=AXIS2_PLACEMENT_3D('',#6635,#5380,#5381);
#4548=AXIS2_PLACEMENT_3D('',#6636,#5382,#5383);
#4549=AXIS2_PLACEMENT_3D('',#6637,#5384,#5385);
#4550=AXIS2_PLACEMENT_3D('',#6646,#5390,#5391);
#4551=AXIS2_PLACEMENT_3D('',#6652,#5395,#5396);
#4552=AXIS2_PLACEMENT_3D('',#6658,#5400,#5401);
#4553=AXIS2_PLACEMENT_3D('',#6661,#5404,#5405);
#4554=AXIS2_PLACEMENT_3D('',#6662,#5406,#5407);
#4555=AXIS2_PLACEMENT_3D('',#6663,#5408,#5409);
#4556=AXIS2_PLACEMENT_3D('',#6664,#5410,#5411);
#4557=AXIS2_PLACEMENT_3D('',#6665,#5412,#5413);
#4558=AXIS2_PLACEMENT_3D('',#6668,#5414,#5415);
#4559=AXIS2_PLACEMENT_3D('',#6669,#5416,#5417);
#4560=AXIS2_PLACEMENT_3D('',#6671,#5418,#5419);
#4561=AXIS2_PLACEMENT_3D('',#6673,#5420,#5421);
#4562=AXIS2_PLACEMENT_3D('',#6674,#5422,#5423);
#4563=AXIS2_PLACEMENT_3D('',#6675,#5424,#5425);
#4564=AXIS2_PLACEMENT_3D('',#6678,#5427,#5428);
#4565=AXIS2_PLACEMENT_3D('',#6679,#5429,#5430);
#4566=AXIS2_PLACEMENT_3D('',#6681,#5431,#5432);
#4567=AXIS2_PLACEMENT_3D('',#6684,#5434,#5435);
#4568=AXIS2_PLACEMENT_3D('',#6685,#5436,#5437);
#4569=AXIS2_PLACEMENT_3D('',#6688,#5439,#5440);
#4570=AXIS2_PLACEMENT_3D('',#6689,#5441,#5442);
#4571=AXIS2_PLACEMENT_3D('',#6690,#5443,#5444);
#4572=AXIS2_PLACEMENT_3D('',#6692,#5445,#5446);
#4573=AXIS2_PLACEMENT_3D('',#6694,#5448,#5449);
#4574=AXIS2_PLACEMENT_3D('',#6696,#5450,#5451);
#4575=AXIS2_PLACEMENT_3D('',#6697,#5452,#5453);
#4576=AXIS2_PLACEMENT_3D('',#6699,#5455,#5456);
#4577=AXIS2_PLACEMENT_3D('',#6700,#5457,#5458);
#4578=AXIS2_PLACEMENT_3D('',#6703,#5459,#5460);
#4579=AXIS2_PLACEMENT_3D('',#6704,#5461,#5462);
#4580=AXIS2_PLACEMENT_3D('',#6706,#5463,#5464);
#4581=AXIS2_PLACEMENT_3D('',#6708,#5465,#5466);
#4582=AXIS2_PLACEMENT_3D('',#6709,#5467,#5468);
#4583=AXIS2_PLACEMENT_3D('',#6710,#5469,#5470);
#4584=AXIS2_PLACEMENT_3D('',#6712,#5471,#5472);
#4585=AXIS2_PLACEMENT_3D('',#6714,#5474,#5475);
#4586=AXIS2_PLACEMENT_3D('',#6716,#5476,#5477);
#4587=AXIS2_PLACEMENT_3D('',#6718,#5478,#5479);
#4588=AXIS2_PLACEMENT_3D('',#6719,#5480,#5481);
#4589=AXIS2_PLACEMENT_3D('',#6721,#5482,#5483);
#4590=AXIS2_PLACEMENT_3D('',#6723,#5485,#5486);
#4591=AXIS2_PLACEMENT_3D('',#6725,#5487,#5488);
#4592=AXIS2_PLACEMENT_3D('',#6727,#5490,#5491);
#4593=AXIS2_PLACEMENT_3D('',#6729,#5492,#5493);
#4594=AXIS2_PLACEMENT_3D('',#6731,#5495,#5496);
#4595=AXIS2_PLACEMENT_3D('',#6732,#5497,#5498);
#4596=AXIS2_PLACEMENT_3D('',#6734,#5500,#5501);
#4597=AXIS2_PLACEMENT_3D('',#6735,#5502,#5503);
#4598=AXIS2_PLACEMENT_3D('',#6738,#5504,#5505);
#4599=AXIS2_PLACEMENT_3D('',#6739,#5506,#5507);
#4600=AXIS2_PLACEMENT_3D('',#6742,#5508,#5509);
#4601=AXIS2_PLACEMENT_3D('',#6743,#5510,#5511);
#4602=AXIS2_PLACEMENT_3D('',#6746,#5512,#5513);
#4603=AXIS2_PLACEMENT_3D('',#6747,#5514,#5515);
#4604=AXIS2_PLACEMENT_3D('',#6750,#5516,#5517);
#4605=AXIS2_PLACEMENT_3D('',#6751,#5518,#5519);
#4606=AXIS2_PLACEMENT_3D('',#6754,#5520,#5521);
#4607=AXIS2_PLACEMENT_3D('',#6755,#5522,#5523);
#4608=AXIS2_PLACEMENT_3D('',#6758,#5524,#5525);
#4609=AXIS2_PLACEMENT_3D('',#6759,#5526,#5527);
#4610=AXIS2_PLACEMENT_3D('',#6762,#5528,#5529);
#4611=AXIS2_PLACEMENT_3D('',#6763,#5530,#5531);
#4612=AXIS2_PLACEMENT_3D('',#6766,#5532,#5533);
#4613=AXIS2_PLACEMENT_3D('',#6767,#5534,#5535);
#4614=AXIS2_PLACEMENT_3D('',#6768,#5536,#5537);
#4615=AXIS2_PLACEMENT_3D('',#6794,#5538,#5539);
#4616=AXIS2_PLACEMENT_3D('',#6818,#5540,#5541);
#4617=AXIS2_PLACEMENT_3D('',#6819,#5542,#5543);
#4618=AXIS2_PLACEMENT_3D('',#6821,#5544,#5545);
#4619=AXIS2_PLACEMENT_3D('',#6846,#5546,#5547);
#4620=AXIS2_PLACEMENT_3D('',#6871,#5548,#5549);
#4621=AXIS2_PLACEMENT_3D('',#6887,#5551,#5552);
#4622=AXIS2_PLACEMENT_3D('',#6902,#5553,#5554);
#4623=AXIS2_PLACEMENT_3D('',#6927,#5555,#5556);
#4624=AXIS2_PLACEMENT_3D('',#6952,#5557,#5558);
#4625=AXIS2_PLACEMENT_3D('',#6977,#5559,#5560);
#4626=AXIS2_PLACEMENT_3D('',#7001,#5561,#5562);
#4627=AXIS2_PLACEMENT_3D('',#7002,#5563,#5564);
#4628=AXIS2_PLACEMENT_3D('',#7004,#5565,#5566);
#4629=AXIS2_PLACEMENT_3D('',#7005,#5567,#5568);
#4630=AXIS2_PLACEMENT_3D('',#7006,#5569,#5570);
#4631=AXIS2_PLACEMENT_3D('',#7030,#5571,#5572);
#4632=AXIS2_PLACEMENT_3D('',#7031,#5573,#5574);
#4633=AXIS2_PLACEMENT_3D('',#7033,#5575,#5576);
#4634=AXIS2_PLACEMENT_3D('',#7034,#5577,#5578);
#4635=AXIS2_PLACEMENT_3D('',#7035,#5579,#5580);
#4636=AXIS2_PLACEMENT_3D('',#7059,#5581,#5582);
#4637=AXIS2_PLACEMENT_3D('',#7060,#5583,#5584);
#4638=AXIS2_PLACEMENT_3D('',#7062,#5585,#5586);
#4639=AXIS2_PLACEMENT_3D('',#7063,#5587,#5588);
#4640=AXIS2_PLACEMENT_3D('',#7064,#5589,#5590);
#4641=AXIS2_PLACEMENT_3D('',#7079,#5591,#5592);
#4642=AXIS2_PLACEMENT_3D('',#7092,#5593,#5594);
#4643=AXIS2_PLACEMENT_3D('',#7094,#5595,#5596);
#4644=AXIS2_PLACEMENT_3D('',#7095,#5597,#5598);
#4645=AXIS2_PLACEMENT_3D('',#7096,#5599,#5600);
#4646=AXIS2_PLACEMENT_3D('',#7120,#5601,#5602);
#4647=AXIS2_PLACEMENT_3D('',#7121,#5603,#5604);
#4648=AXIS2_PLACEMENT_3D('',#7123,#5605,#5606);
#4649=AXIS2_PLACEMENT_3D('',#7124,#5607,#5608);
#4650=AXIS2_PLACEMENT_3D('',#7125,#5609,#5610);
#4651=AXIS2_PLACEMENT_3D('',#7149,#5611,#5612);
#4652=AXIS2_PLACEMENT_3D('',#7150,#5613,#5614);
#4653=AXIS2_PLACEMENT_3D('',#7152,#5615,#5616);
#4654=AXIS2_PLACEMENT_3D('',#7153,#5617,#5618);
#4655=AXIS2_PLACEMENT_3D('',#7154,#5619,#5620);
#4656=AXIS2_PLACEMENT_3D('',#7178,#5621,#5622);
#4657=AXIS2_PLACEMENT_3D('',#7179,#5623,#5624);
#4658=AXIS2_PLACEMENT_3D('',#7181,#5625,#5626);
#4659=AXIS2_PLACEMENT_3D('',#7184,#5628,#5629);
#4660=AXIS2_PLACEMENT_3D('',#7208,#5630,#5631);
#4661=AXIS2_PLACEMENT_3D('',#7209,#5632,#5633);
#4662=AXIS2_PLACEMENT_3D('',#7210,#5634,#5635);
#4663=AXIS2_PLACEMENT_3D('',#7211,#5636,#5637);
#4664=AXIS2_PLACEMENT_3D('',#7212,#5638,#5639);
#4665=AXIS2_PLACEMENT_3D('',#7213,#5640,#5641);
#4666=AXIS2_PLACEMENT_3D('',#7214,#5642,#5643);
#4667=AXIS2_PLACEMENT_3D('',#7215,#5644,#5645);
#4668=AXIS2_PLACEMENT_3D('',#7216,#5646,#5647);
#4669=AXIS2_PLACEMENT_3D('',#7218,#5648,#5649);
#4670=AXIS2_PLACEMENT_3D('',#7220,#5650,#5651);
#4671=AXIS2_PLACEMENT_3D('',#7221,#5652,#5653);
#4672=AXIS2_PLACEMENT_3D('',#7223,#5654,#5655);
#4673=AXIS2_PLACEMENT_3D('',#7225,#5657,#5658);
#4674=AXIS2_PLACEMENT_3D('',#7227,#5659,#5660);
#4675=AXIS2_PLACEMENT_3D('',#7228,#5661,#5662);
#4676=AXIS2_PLACEMENT_3D('',#7230,#5664,#5665);
#4677=AXIS2_PLACEMENT_3D('',#7232,#5666,#5667);
#4678=AXIS2_PLACEMENT_3D('',#7234,#5668,#5669);
#4679=AXIS2_PLACEMENT_3D('',#7235,#5670,#5671);
#4680=AXIS2_PLACEMENT_3D('',#7237,#5672,#5673);
#4681=AXIS2_PLACEMENT_3D('',#7239,#5675,#5676);
#4682=AXIS2_PLACEMENT_3D('',#7241,#5677,#5678);
#4683=AXIS2_PLACEMENT_3D('',#7242,#5679,#5680);
#4684=AXIS2_PLACEMENT_3D('',#7244,#5682,#5683);
#4685=AXIS2_PLACEMENT_3D('',#7245,#5684,#5685);
#4686=AXIS2_PLACEMENT_3D('',#7246,#5686,#5687);
#4687=AXIS2_PLACEMENT_3D('',#7247,#5688,#5689);
#4688=AXIS2_PLACEMENT_3D('',#7248,#5690,#5691);
#4689=AXIS2_PLACEMENT_3D('',#7249,#5692,#5693);
#4690=AXIS2_PLACEMENT_3D('',#7250,#5694,#5695);
#4691=AXIS2_PLACEMENT_3D('',#7252,#5696,#5697);
#4692=AXIS2_PLACEMENT_3D('',#7253,#5698,#5699);
#4693=AXIS2_PLACEMENT_3D('',#7255,#5700,#5701);
#4694=AXIS2_PLACEMENT_3D('',#7257,#5703,#5704);
#4695=AXIS2_PLACEMENT_3D('',#7259,#5705,#5706);
#4696=AXIS2_PLACEMENT_3D('',#7261,#5708,#5709);
#4697=AXIS2_PLACEMENT_3D('',#7263,#5710,#5711);
#4698=AXIS2_PLACEMENT_3D('',#7265,#5713,#5714);
#4699=AXIS2_PLACEMENT_3D('',#7267,#5715,#5716);
#4700=AXIS2_PLACEMENT_3D('',#7268,#5717,#5718);
#4701=AXIS2_PLACEMENT_3D('',#7270,#5719,#5720);
#4702=AXIS2_PLACEMENT_3D('',#7272,#5722,#5723);
#4703=AXIS2_PLACEMENT_3D('',#7274,#5724,#5725);
#4704=AXIS2_PLACEMENT_3D('',#7276,#5727,#5728);
#4705=AXIS2_PLACEMENT_3D('',#7278,#5729,#5730);
#4706=AXIS2_PLACEMENT_3D('',#7280,#5732,#5733);
#4707=AXIS2_PLACEMENT_3D('',#7281,#5734,#5735);
#4708=AXIS2_PLACEMENT_3D('',#7290,#5740,#5741);
#4709=AXIS2_PLACEMENT_3D('',#7296,#5745,#5746);
#4710=AXIS2_PLACEMENT_3D('',#7302,#5750,#5751);
#4711=AXIS2_PLACEMENT_3D('',#7308,#5755,#5756);
#4712=AXIS2_PLACEMENT_3D('',#7314,#5760,#5761);
#4713=AXIS2_PLACEMENT_3D('',#7317,#5764,#5765);
#4714=AXIS2_PLACEMENT_3D('',#7318,#5766,#5767);
#4715=AXIS2_PLACEMENT_3D('',#7319,#5768,#5769);
#4716=AXIS2_PLACEMENT_3D('',#7320,#5770,#5771);
#4717=AXIS2_PLACEMENT_3D('',#7322,#5772,#5773);
#4718=AXIS2_PLACEMENT_3D('',#7323,#5774,#5775);
#4719=AXIS2_PLACEMENT_3D('',#7325,#5776,#5777);
#4720=AXIS2_PLACEMENT_3D('',#7327,#5779,#5780);
#4721=AXIS2_PLACEMENT_3D('',#7329,#5781,#5782);
#4722=AXIS2_PLACEMENT_3D('',#7331,#5784,#5785);
#4723=AXIS2_PLACEMENT_3D('',#7333,#5786,#5787);
#4724=AXIS2_PLACEMENT_3D('',#7335,#5789,#5790);
#4725=AXIS2_PLACEMENT_3D('',#7337,#5791,#5792);
#4726=AXIS2_PLACEMENT_3D('',#7338,#5793,#5794);
#4727=AXIS2_PLACEMENT_3D('',#7340,#5795,#5796);
#4728=AXIS2_PLACEMENT_3D('',#7342,#5798,#5799);
#4729=AXIS2_PLACEMENT_3D('',#7344,#5800,#5801);
#4730=AXIS2_PLACEMENT_3D('',#7346,#5803,#5804);
#4731=AXIS2_PLACEMENT_3D('',#7348,#5805,#5806);
#4732=AXIS2_PLACEMENT_3D('',#7350,#5808,#5809);
#4733=AXIS2_PLACEMENT_3D('',#7351,#5810,#5811);
#4734=AXIS2_PLACEMENT_3D('',#7360,#5816,#5817);
#4735=AXIS2_PLACEMENT_3D('',#7366,#5821,#5822);
#4736=AXIS2_PLACEMENT_3D('',#7372,#5826,#5827);
#4737=AXIS2_PLACEMENT_3D('',#7378,#5831,#5832);
#4738=AXIS2_PLACEMENT_3D('',#7384,#5836,#5837);
#4739=AXIS2_PLACEMENT_3D('',#7387,#5840,#5841);
#4740=AXIS2_PLACEMENT_3D('',#7388,#5842,#5843);
#4741=AXIS2_PLACEMENT_3D('',#7389,#5844,#5845);
#4742=AXIS2_PLACEMENT_3D('',#7390,#5846,#5847);
#4743=AXIS2_PLACEMENT_3D('',#7391,#5848,#5849);
#4744=AXIS2_PLACEMENT_3D('',#7392,#5850,#5851);
#4745=AXIS2_PLACEMENT_3D('',#7393,#5852,#5853);
#4746=AXIS2_PLACEMENT_3D('',#7394,#5854,#5855);
#4747=AXIS2_PLACEMENT_3D('',#7395,#5856,#5857);
#4748=AXIS2_PLACEMENT_3D('',#7396,#5858,#5859);
#4749=AXIS2_PLACEMENT_3D('',#7397,#5860,#5861);
#4750=AXIS2_PLACEMENT_3D('',#7398,#5862,#5863);
#4751=AXIS2_PLACEMENT_3D('',#7399,#5864,#5865);
#4752=AXIS2_PLACEMENT_3D('',#7400,#5866,#5867);
#4753=AXIS2_PLACEMENT_3D('',#7401,#5868,#5869);
#4754=AXIS2_PLACEMENT_3D('',#7402,#5870,#5871);
#4755=AXIS2_PLACEMENT_3D('',#7403,#5872,#5873);
#4756=AXIS2_PLACEMENT_3D('',#7404,#5874,#5875);
#4757=AXIS2_PLACEMENT_3D('',#7405,#5876,#5877);
#4758=AXIS2_PLACEMENT_3D('',#7406,#5878,#5879);
#4759=AXIS2_PLACEMENT_3D('',#7407,#5880,#5881);
#4760=AXIS2_PLACEMENT_3D('',#7408,#5882,#5883);
#4761=AXIS2_PLACEMENT_3D('',#7409,#5884,#5885);
#4762=AXIS2_PLACEMENT_3D('',#7410,#5886,#5887);
#4763=AXIS2_PLACEMENT_3D('',#7411,#5888,#5889);
#4764=AXIS2_PLACEMENT_3D('',#7412,#5890,#5891);
#4765=AXIS2_PLACEMENT_3D('',#7413,#5892,#5893);
#4766=AXIS2_PLACEMENT_3D('',#7422,#5898,#5899);
#4767=AXIS2_PLACEMENT_3D('',#7424,#5900,#5901);
#4768=AXIS2_PLACEMENT_3D('',#7428,#5904,#5905);
#4769=AXIS2_PLACEMENT_3D('',#7434,#5909,#5910);
#4770=AXIS2_PLACEMENT_3D('',#7436,#5912,#5913);
#4771=AXIS2_PLACEMENT_3D('',#7437,#5914,#5915);
#4772=AXIS2_PLACEMENT_3D('',#7438,#5916,#5917);
#4773=AXIS2_PLACEMENT_3D('',#7440,#5918,#5919);
#4774=AXIS2_PLACEMENT_3D('',#7442,#5920,#5921);
#4775=AXIS2_PLACEMENT_3D('',#7443,#5922,#5923);
#4776=AXIS2_PLACEMENT_3D('',#7445,#5924,#5925);
#4777=AXIS2_PLACEMENT_3D('',#7447,#5926,#5927);
#4778=AXIS2_PLACEMENT_3D('',#7448,#5928,#5929);
#4779=AXIS2_PLACEMENT_3D('',#7450,#5931,#5932);
#4780=AXIS2_PLACEMENT_3D('',#7453,#5934,#5935);
#4781=AXIS2_PLACEMENT_3D('',#7454,#5936,#5937);
#4782=AXIS2_PLACEMENT_3D('',#7456,#5938,#5939);
#4783=AXIS2_PLACEMENT_3D('',#7458,#5941,#5942);
#4784=AXIS2_PLACEMENT_3D('',#7459,#5943,#5944);
#4785=AXIS2_PLACEMENT_3D('',#7460,#5945,#5946);
#4786=AXIS2_PLACEMENT_3D('',#7461,#5947,#5948);
#4787=AXIS2_PLACEMENT_3D('',#7463,#5949,#5950);
#4788=AXIS2_PLACEMENT_3D('',#7466,#5952,#5953);
#4789=AXIS2_PLACEMENT_3D('',#7467,#5954,#5955);
#4790=AXIS2_PLACEMENT_3D('',#7469,#5956,#5957);
#4791=AXIS2_PLACEMENT_3D('',#7472,#5959,#5960);
#4792=AXIS2_PLACEMENT_3D('',#7473,#5961,#5962);
#4793=AXIS2_PLACEMENT_3D('',#7474,#5963,#5964);
#4794=AXIS2_PLACEMENT_3D('',#7475,#5965,#5966);
#4795=AXIS2_PLACEMENT_3D('',#7476,#5967,#5968);
#4796=AXIS2_PLACEMENT_3D('',#7480,#5970,#5971);
#4797=AXIS2_PLACEMENT_3D('',#7481,#5972,#5973);
#4798=AXIS2_PLACEMENT_3D('',#7498,#5974,#5975);
#4799=AXIS2_PLACEMENT_3D('',#7539,#5977,#5978);
#4800=AXIS2_PLACEMENT_3D('',#7554,#5979,#5980);
#4801=AXIS2_PLACEMENT_3D('',#7556,#5982,#5983);
#4802=AXIS2_PLACEMENT_3D('',#7558,#5984,#5985);
#4803=AXIS2_PLACEMENT_3D('',#7561,#5987,#5988);
#4804=AXIS2_PLACEMENT_3D('',#7562,#5989,#5990);
#4805=AXIS2_PLACEMENT_3D('',#7564,#5991,#5992);
#4806=AXIS2_PLACEMENT_3D('',#7567,#5994,#5995);
#4807=AXIS2_PLACEMENT_3D('',#7568,#5996,#5997);
#4808=AXIS2_PLACEMENT_3D('',#7569,#5998,#5999);
#4809=AXIS2_PLACEMENT_3D('',#7570,#6000,#6001);
#4810=AXIS2_PLACEMENT_3D('',#7571,#6002,#6003);
#4811=AXIS2_PLACEMENT_3D('',#7575,#6005,#6006);
#4812=AXIS2_PLACEMENT_3D('',#7576,#6007,#6008);
#4813=AXIS2_PLACEMENT_3D('',#7589,#6009,#6010);
#4814=AXIS2_PLACEMENT_3D('',#7630,#6012,#6013);
#4815=AXIS2_PLACEMENT_3D('',#7641,#6014,#6015);
#4816=AXIS2_PLACEMENT_3D('',#7643,#6017,#6018);
#4817=AXIS2_PLACEMENT_3D('',#7652,#6023,#6024);
#4818=AXIS2_PLACEMENT_3D('',#7658,#6028,#6029);
#4819=AXIS2_PLACEMENT_3D('',#7664,#6033,#6034);
#4820=AXIS2_PLACEMENT_3D('',#7666,#6035,#6036);
#4821=AXIS2_PLACEMENT_3D('',#7667,#6037,#6038);
#4822=AXIS2_PLACEMENT_3D('',#7668,#6039,#6040);
#4823=AXIS2_PLACEMENT_3D('',#7669,#6041,#6042);
#4824=AXIS2_PLACEMENT_3D('',#7670,#6043,#6044);
#4825=AXIS2_PLACEMENT_3D('',#7672,#6045,#6046);
#4826=AXIS2_PLACEMENT_3D('',#7675,#6048,#6049);
#4827=AXIS2_PLACEMENT_3D('',#7676,#6050,#6051);
#4828=AXIS2_PLACEMENT_3D('',#7678,#6052,#6053);
#4829=AXIS2_PLACEMENT_3D('',#7681,#6055,#6056);
#4830=AXIS2_PLACEMENT_3D('',#7682,#6057,#6058);
#4831=AXIS2_PLACEMENT_3D('',#7684,#6059,#6060);
#4832=AXIS2_PLACEMENT_3D('',#7687,#6062,#6063);
#4833=AXIS2_PLACEMENT_3D('',#7688,#6064,#6065);
#4834=AXIS2_PLACEMENT_3D('',#7690,#6066,#6067);
#4835=AXIS2_PLACEMENT_3D('',#7693,#6069,#6070);
#4836=AXIS2_PLACEMENT_3D('',#7694,#6071,#6072);
#4837=AXIS2_PLACEMENT_3D('',#7696,#6073,#6074);
#4838=AXIS2_PLACEMENT_3D('',#7698,#6075,#6076);
#4839=AXIS2_PLACEMENT_3D('',#7699,#6077,#6078);
#4840=AXIS2_PLACEMENT_3D('',#7702,#6080,#6081);
#4841=AXIS2_PLACEMENT_3D('',#7703,#6082,#6083);
#4842=AXIS2_PLACEMENT_3D('',#7705,#6085,#6086);
#4843=AXIS2_PLACEMENT_3D('',#7706,#6087,#6088);
#4844=AXIS2_PLACEMENT_3D('',#7707,#6089,#6090);
#4845=AXIS2_PLACEMENT_3D('',#7724,#6099,#6100);
#4846=AXIS2_PLACEMENT_3D('',#7730,#6104,#6105);
#4847=AXIS2_PLACEMENT_3D('',#7734,#6108,#6109);
#4848=AXIS2_PLACEMENT_3D('',#7738,#6112,#6113);
#4849=AXIS2_PLACEMENT_3D('',#7742,#6116,#6117);
#4850=AXIS2_PLACEMENT_3D('',#7750,#6122,#6123);
#4851=AXIS2_PLACEMENT_3D('',#7752,#6125,#6126);
#4852=AXIS2_PLACEMENT_3D('',#7754,#6128,#6129);
#4853=AXIS2_PLACEMENT_3D('',#7756,#6131,#6132);
#4854=AXIS2_PLACEMENT_3D('',#7757,#6133,#6134);
#4855=AXIS2_PLACEMENT_3D('',#7758,#6135,#6136);
#4856=AXIS2_PLACEMENT_3D('',#7767,#6141,#6142);
#4857=AXIS2_PLACEMENT_3D('',#7773,#6146,#6147);
#4858=AXIS2_PLACEMENT_3D('',#7779,#6151,#6152);
#4859=AXIS2_PLACEMENT_3D('',#7785,#6156,#6157);
#4860=AXIS2_PLACEMENT_3D('',#7791,#6161,#6162);
#4861=AXIS2_PLACEMENT_3D('',#7794,#6165,#6166);
#4862=AXIS2_PLACEMENT_3D('',#7795,#6167,#6168);
#4863=AXIS2_PLACEMENT_3D('',#7797,#6169,#6170);
#4864=AXIS2_PLACEMENT_3D('',#7798,#6171,#6172);
#4865=AXIS2_PLACEMENT_3D('',#7800,#6173,#6174);
#4866=AXIS2_PLACEMENT_3D('',#7802,#6176,#6177);
#4867=AXIS2_PLACEMENT_3D('',#7804,#6178,#6179);
#4868=AXIS2_PLACEMENT_3D('',#7806,#6181,#6182);
#4869=AXIS2_PLACEMENT_3D('',#7808,#6183,#6184);
#4870=AXIS2_PLACEMENT_3D('',#7810,#6186,#6187);
#4871=AXIS2_PLACEMENT_3D('',#7811,#6188,#6189);
#4872=AXIS2_PLACEMENT_3D('',#7812,#6190,#6191);
#4873=AXIS2_PLACEMENT_3D('',#7813,#6192,#6193);
#4874=AXIS2_PLACEMENT_3D('',#7814,#6194,#6195);
#4875=AXIS2_PLACEMENT_3D('',#7815,#6196,#6197);
#4876=AXIS2_PLACEMENT_3D('',#7816,#6198,#6199);
#4877=AXIS2_PLACEMENT_3D('',#7817,#6200,#6201);
#4878=AXIS2_PLACEMENT_3D('',#7818,#6202,#6203);
#4879=AXIS2_PLACEMENT_3D('',#7819,#6204,#6205);
#4880=DIRECTION('axis',(0.,0.,1.));
#4881=DIRECTION('refdir',(1.,0.,0.));
#4882=DIRECTION('axis',(0.,0.,1.));
#4883=DIRECTION('refdir',(1.,0.,0.));
#4884=DIRECTION('axis',(0.,0.,1.));
#4885=DIRECTION('refdir',(1.,0.,0.));
#4886=DIRECTION('center_axis',(0.,0.,1.));
#4887=DIRECTION('ref_axis',(1.,0.,0.));
#4888=DIRECTION('center_axis',(0.,0.,1.));
#4889=DIRECTION('ref_axis',(1.,0.,0.));
#4890=DIRECTION('',(0.,0.,1.));
#4891=DIRECTION('center_axis',(0.,0.,-1.));
#4892=DIRECTION('ref_axis',(1.,0.,0.));
#4893=DIRECTION('center_axis',(0.,0.,1.));
#4894=DIRECTION('ref_axis',(1.,0.,0.));
#4895=DIRECTION('center_axis',(0.,0.,1.));
#4896=DIRECTION('ref_axis',(1.,0.,0.));
#4897=DIRECTION('',(0.,0.,1.));
#4898=DIRECTION('center_axis',(0.,0.,-1.));
#4899=DIRECTION('ref_axis',(1.,0.,0.));
#4900=DIRECTION('center_axis',(0.,0.,1.));
#4901=DIRECTION('ref_axis',(1.,0.,0.));
#4902=DIRECTION('center_axis',(0.,0.,1.));
#4903=DIRECTION('ref_axis',(1.,0.,0.));
#4904=DIRECTION('',(0.,0.,1.));
#4905=DIRECTION('center_axis',(0.,0.,-1.));
#4906=DIRECTION('ref_axis',(1.,0.,0.));
#4907=DIRECTION('center_axis',(0.,0.,1.));
#4908=DIRECTION('ref_axis',(1.,0.,0.));
#4909=DIRECTION('center_axis',(0.,0.,1.));
#4910=DIRECTION('ref_axis',(1.,0.,0.));
#4911=DIRECTION('',(0.,0.,1.));
#4912=DIRECTION('center_axis',(0.,0.,-1.));
#4913=DIRECTION('ref_axis',(1.,0.,0.));
#4914=DIRECTION('center_axis',(0.,1.,0.));
#4915=DIRECTION('ref_axis',(-1.,0.,0.));
#4916=DIRECTION('',(-1.,0.,0.));
#4917=DIRECTION('',(0.,0.,1.));
#4918=DIRECTION('',(-1.,0.,0.));
#4919=DIRECTION('',(0.,0.,1.));
#4920=DIRECTION('center_axis',(1.,0.,0.));
#4921=DIRECTION('ref_axis',(0.,1.,0.));
#4922=DIRECTION('',(0.,1.,0.));
#4923=DIRECTION('',(0.,1.,0.));
#4924=DIRECTION('',(0.,0.,1.));
#4925=DIRECTION('center_axis',(0.,-1.,0.));
#4926=DIRECTION('ref_axis',(1.,0.,0.));
#4927=DIRECTION('',(1.,0.,0.));
#4928=DIRECTION('',(1.,0.,0.));
#4929=DIRECTION('',(0.,0.,1.));
#4930=DIRECTION('center_axis',(-1.,0.,0.));
#4931=DIRECTION('ref_axis',(0.,-1.,0.));
#4932=DIRECTION('',(0.,-1.,0.));
#4933=DIRECTION('',(0.,-1.,0.));
#4934=DIRECTION('center_axis',(0.,0.,1.));
#4935=DIRECTION('ref_axis',(1.,0.,0.));
#4936=DIRECTION('center_axis',(0.,0.,1.));
#4937=DIRECTION('ref_axis',(1.,0.,0.));
#4938=DIRECTION('axis',(0.,0.,1.));
#4939=DIRECTION('refdir',(1.,0.,0.));
#4940=DIRECTION('center_axis',(0.,1.,0.));
#4941=DIRECTION('ref_axis',(1.,0.,0.));
#4942=DIRECTION('center_axis',(0.,1.,0.));
#4943=DIRECTION('ref_axis',(1.,0.,0.));
#4944=DIRECTION('',(0.,1.,0.));
#4945=DIRECTION('center_axis',(0.,-1.,0.));
#4946=DIRECTION('ref_axis',(1.,0.,0.));
#4947=DIRECTION('center_axis',(0.,1.,0.));
#4948=DIRECTION('ref_axis',(1.,0.,0.));
#4949=DIRECTION('center_axis',(0.,1.,0.));
#4950=DIRECTION('ref_axis',(1.,0.,0.));
#4951=DIRECTION('center_axis',(0.,1.,0.));
#4952=DIRECTION('ref_axis',(1.,0.,0.));
#4953=DIRECTION('',(0.,1.,0.));
#4954=DIRECTION('center_axis',(0.,-1.,0.));
#4955=DIRECTION('ref_axis',(1.,0.,0.));
#4956=DIRECTION('center_axis',(0.,1.,0.));
#4957=DIRECTION('ref_axis',(1.,0.,0.));
#4958=DIRECTION('center_axis',(0.,1.,0.));
#4959=DIRECTION('ref_axis',(1.,0.,0.));
#4960=DIRECTION('center_axis',(0.,1.,0.));
#4961=DIRECTION('ref_axis',(1.,0.,0.));
#4962=DIRECTION('',(0.,1.,0.));
#4963=DIRECTION('center_axis',(0.,-1.,0.));
#4964=DIRECTION('ref_axis',(1.,0.,0.));
#4965=DIRECTION('center_axis',(0.,1.,0.));
#4966=DIRECTION('ref_axis',(1.,0.,0.));
#4967=DIRECTION('center_axis',(0.,1.,0.));
#4968=DIRECTION('ref_axis',(1.,0.,0.));
#4969=DIRECTION('center_axis',(0.,1.,0.));
#4970=DIRECTION('ref_axis',(1.,0.,0.));
#4971=DIRECTION('',(0.,1.,0.));
#4972=DIRECTION('center_axis',(0.,-1.,0.));
#4973=DIRECTION('ref_axis',(1.,0.,0.));
#4974=DIRECTION('center_axis',(0.,1.,0.));
#4975=DIRECTION('ref_axis',(1.,0.,0.));
#4976=DIRECTION('center_axis',(0.,1.,0.));
#4977=DIRECTION('ref_axis',(1.,0.,0.));
#4978=DIRECTION('center_axis',(0.,1.,0.));
#4979=DIRECTION('ref_axis',(1.,0.,0.));
#4980=DIRECTION('',(0.,1.,0.));
#4981=DIRECTION('center_axis',(0.,1.,0.));
#4982=DIRECTION('ref_axis',(1.,0.,0.));
#4983=DIRECTION('center_axis',(0.,1.,0.));
#4984=DIRECTION('ref_axis',(1.,0.,0.));
#4985=DIRECTION('center_axis',(0.,1.,0.));
#4986=DIRECTION('ref_axis',(1.,0.,0.));
#4987=DIRECTION('center_axis',(0.,1.,0.));
#4988=DIRECTION('ref_axis',(1.,0.,0.));
#4989=DIRECTION('',(0.,1.,0.));
#4990=DIRECTION('center_axis',(0.,1.,0.));
#4991=DIRECTION('ref_axis',(1.,0.,0.));
#4992=DIRECTION('center_axis',(0.,1.,0.));
#4993=DIRECTION('ref_axis',(1.,0.,0.));
#4994=DIRECTION('center_axis',(0.,1.,0.));
#4995=DIRECTION('ref_axis',(1.,0.,0.));
#4996=DIRECTION('center_axis',(0.,1.,0.));
#4997=DIRECTION('ref_axis',(1.,0.,0.));
#4998=DIRECTION('',(0.,1.,0.));
#4999=DIRECTION('center_axis',(0.,1.,0.));
#5000=DIRECTION('ref_axis',(1.,0.,0.));
#5001=DIRECTION('center_axis',(0.,1.,0.));
#5002=DIRECTION('ref_axis',(1.,0.,0.));
#5003=DIRECTION('center_axis',(0.,1.,0.));
#5004=DIRECTION('ref_axis',(1.,0.,0.));
#5005=DIRECTION('center_axis',(0.,1.,0.));
#5006=DIRECTION('ref_axis',(1.,0.,0.));
#5007=DIRECTION('',(0.,1.,0.));
#5008=DIRECTION('center_axis',(0.,1.,0.));
#5009=DIRECTION('ref_axis',(1.,0.,0.));
#5010=DIRECTION('center_axis',(0.,1.,0.));
#5011=DIRECTION('ref_axis',(1.,0.,0.));
#5012=DIRECTION('center_axis',(0.,0.,1.));
#5013=DIRECTION('ref_axis',(1.,0.,0.));
#5014=DIRECTION('center_axis',(0.,0.,1.));
#5015=DIRECTION('ref_axis',(1.,0.,0.));
#5016=DIRECTION('',(0.,0.,1.));
#5017=DIRECTION('center_axis',(0.,0.,-1.));
#5018=DIRECTION('ref_axis',(1.,0.,0.));
#5019=DIRECTION('center_axis',(0.,0.,1.));
#5020=DIRECTION('ref_axis',(1.,0.,0.));
#5021=DIRECTION('center_axis',(0.,0.,1.));
#5022=DIRECTION('ref_axis',(1.,0.,0.));
#5023=DIRECTION('',(0.,0.,1.));
#5024=DIRECTION('center_axis',(0.,0.,-1.));
#5025=DIRECTION('ref_axis',(1.,0.,0.));
#5026=DIRECTION('center_axis',(0.,0.,1.));
#5027=DIRECTION('ref_axis',(1.,0.,0.));
#5028=DIRECTION('center_axis',(0.,0.,1.));
#5029=DIRECTION('ref_axis',(1.,0.,0.));
#5030=DIRECTION('',(0.,0.,1.));
#5031=DIRECTION('center_axis',(0.,0.,-1.));
#5032=DIRECTION('ref_axis',(1.,0.,0.));
#5033=DIRECTION('center_axis',(0.,0.,1.));
#5034=DIRECTION('ref_axis',(1.,0.,0.));
#5035=DIRECTION('center_axis',(0.,0.,1.));
#5036=DIRECTION('ref_axis',(1.,0.,0.));
#5037=DIRECTION('',(0.,0.,1.));
#5038=DIRECTION('center_axis',(0.,0.,-1.));
#5039=DIRECTION('ref_axis',(1.,0.,0.));
#5040=DIRECTION('center_axis',(0.,1.,0.));
#5041=DIRECTION('ref_axis',(0.,0.,1.));
#5042=DIRECTION('center_axis',(0.,1.,0.));
#5043=DIRECTION('ref_axis',(1.,0.,0.));
#5044=DIRECTION('',(1.,0.,0.));
#5045=DIRECTION('',(0.,0.,-1.));
#5046=DIRECTION('',(-1.,0.,0.));
#5047=DIRECTION('center_axis',(0.,1.,0.));
#5048=DIRECTION('ref_axis',(0.,0.,1.));
#5049=DIRECTION('center_axis',(0.,1.,0.));
#5050=DIRECTION('ref_axis',(1.,0.,0.));
#5051=DIRECTION('',(-1.,0.,0.));
#5052=DIRECTION('',(0.,0.,1.));
#5053=DIRECTION('',(1.,0.,0.));
#5054=DIRECTION('center_axis',(0.,1.,0.));
#5055=DIRECTION('ref_axis',(1.,0.,0.));
#5056=DIRECTION('center_axis',(0.,-1.,0.));
#5057=DIRECTION('ref_axis',(1.,0.,0.));
#5058=DIRECTION('',(1.,0.,0.));
#5059=DIRECTION('',(0.,0.,1.));
#5060=DIRECTION('',(-1.,0.,0.));
#5061=DIRECTION('center_axis',(0.,1.,0.));
#5062=DIRECTION('ref_axis',(1.,0.,0.));
#5063=DIRECTION('center_axis',(0.,-1.,0.));
#5064=DIRECTION('ref_axis',(1.,0.,0.));
#5065=DIRECTION('',(-1.,0.,0.));
#5066=DIRECTION('',(0.,0.,-1.));
#5067=DIRECTION('',(1.,0.,0.));
#5068=DIRECTION('center_axis',(0.,0.,1.));
#5069=DIRECTION('ref_axis',(1.,0.,0.));
#5070=DIRECTION('',(0.,1.,0.));
#5071=DIRECTION('',(0.,1.,0.));
#5072=DIRECTION('center_axis',(0.,0.,1.));
#5073=DIRECTION('ref_axis',(1.,0.,0.));
#5074=DIRECTION('',(0.,-1.,0.));
#5075=DIRECTION('',(0.,1.,0.));
#5076=DIRECTION('center_axis',(-1.,0.,0.));
#5077=DIRECTION('ref_axis',(0.,0.,1.));
#5078=DIRECTION('',(0.,1.,0.));
#5079=DIRECTION('center_axis',(0.,0.,-1.));
#5080=DIRECTION('ref_axis',(-1.,0.,0.));
#5081=DIRECTION('',(0.,1.,0.));
#5082=DIRECTION('center_axis',(1.,0.,0.));
#5083=DIRECTION('ref_axis',(0.,0.,-1.));
#5084=DIRECTION('center_axis',(0.,1.,0.));
#5085=DIRECTION('ref_axis',(0.,0.,1.));
#5086=DIRECTION('center_axis',(0.,1.,0.));
#5087=DIRECTION('ref_axis',(1.,0.,0.));
#5088=DIRECTION('',(1.,0.,0.));
#5089=DIRECTION('',(0.,0.,-1.));
#5090=DIRECTION('',(-1.,0.,0.));
#5091=DIRECTION('center_axis',(0.,1.,0.));
#5092=DIRECTION('ref_axis',(0.,0.,1.));
#5093=DIRECTION('center_axis',(0.,1.,0.));
#5094=DIRECTION('ref_axis',(1.,0.,0.));
#5095=DIRECTION('',(-1.,0.,0.));
#5096=DIRECTION('',(0.,0.,1.));
#5097=DIRECTION('',(1.,0.,0.));
#5098=DIRECTION('center_axis',(0.,1.,0.));
#5099=DIRECTION('ref_axis',(1.,0.,0.));
#5100=DIRECTION('center_axis',(0.,-1.,0.));
#5101=DIRECTION('ref_axis',(1.,0.,0.));
#5102=DIRECTION('',(1.,0.,0.));
#5103=DIRECTION('',(0.,0.,1.));
#5104=DIRECTION('',(-1.,0.,0.));
#5105=DIRECTION('center_axis',(0.,1.,0.));
#5106=DIRECTION('ref_axis',(1.,0.,0.));
#5107=DIRECTION('center_axis',(0.,-1.,0.));
#5108=DIRECTION('ref_axis',(1.,0.,0.));
#5109=DIRECTION('',(-1.,0.,0.));
#5110=DIRECTION('',(0.,0.,-1.));
#5111=DIRECTION('',(1.,0.,0.));
#5112=DIRECTION('center_axis',(0.,0.,1.));
#5113=DIRECTION('ref_axis',(1.,0.,0.));
#5114=DIRECTION('',(0.,1.,0.));
#5115=DIRECTION('',(0.,1.,0.));
#5116=DIRECTION('center_axis',(0.,0.,1.));
#5117=DIRECTION('ref_axis',(1.,0.,0.));
#5118=DIRECTION('',(0.,-1.,0.));
#5119=DIRECTION('',(0.,1.,0.));
#5120=DIRECTION('center_axis',(-1.,0.,0.));
#5121=DIRECTION('ref_axis',(0.,0.,1.));
#5122=DIRECTION('',(0.,1.,0.));
#5123=DIRECTION('center_axis',(0.,0.,-1.));
#5124=DIRECTION('ref_axis',(-1.,0.,0.));
#5125=DIRECTION('',(0.,1.,0.));
#5126=DIRECTION('center_axis',(1.,0.,0.));
#5127=DIRECTION('ref_axis',(0.,0.,-1.));
#5128=DIRECTION('center_axis',(0.,1.,0.));
#5129=DIRECTION('ref_axis',(1.,0.,0.));
#5130=DIRECTION('center_axis',(0.,-1.,0.));
#5131=DIRECTION('ref_axis',(1.,0.,0.));
#5132=DIRECTION('',(0.,-1.,0.));
#5133=DIRECTION('center_axis',(0.,-1.,0.));
#5134=DIRECTION('ref_axis',(1.,0.,0.));
#5135=DIRECTION('center_axis',(0.,1.,0.));
#5136=DIRECTION('ref_axis',(1.,0.,0.));
#5137=DIRECTION('center_axis',(0.,1.,0.));
#5138=DIRECTION('ref_axis',(1.,0.,0.));
#5139=DIRECTION('',(0.,-1.,0.));
#5140=DIRECTION('center_axis',(0.,1.,0.));
#5141=DIRECTION('ref_axis',(1.,0.,0.));
#5142=DIRECTION('center_axis',(0.,1.,0.));
#5143=DIRECTION('ref_axis',(1.,0.,0.));
#5144=DIRECTION('center_axis',(0.,1.,0.));
#5145=DIRECTION('ref_axis',(1.,0.,0.));
#5146=DIRECTION('axis',(0.,0.,1.));
#5147=DIRECTION('refdir',(1.,0.,0.));
#5148=DIRECTION('center_axis',(0.,1.,0.));
#5149=DIRECTION('ref_axis',(1.,0.,0.));
#5150=DIRECTION('center_axis',(0.,-1.,0.));
#5151=DIRECTION('ref_axis',(1.,0.,0.));
#5152=DIRECTION('',(0.,-1.,0.));
#5153=DIRECTION('center_axis',(0.,-1.,0.));
#5154=DIRECTION('ref_axis',(1.,0.,0.));
#5155=DIRECTION('center_axis',(0.,1.,0.));
#5156=DIRECTION('ref_axis',(1.,0.,0.));
#5157=DIRECTION('center_axis',(0.,1.,0.));
#5158=DIRECTION('ref_axis',(1.,0.,0.));
#5159=DIRECTION('',(0.,-1.,0.));
#5160=DIRECTION('center_axis',(0.,1.,0.));
#5161=DIRECTION('ref_axis',(1.,0.,0.));
#5162=DIRECTION('center_axis',(0.,1.,0.));
#5163=DIRECTION('ref_axis',(1.,0.,0.));
#5164=DIRECTION('center_axis',(0.,1.,0.));
#5165=DIRECTION('ref_axis',(1.,0.,0.));
#5166=DIRECTION('axis',(0.,0.,1.));
#5167=DIRECTION('refdir',(1.,0.,0.));
#5168=DIRECTION('center_axis',(0.,1.,0.));
#5169=DIRECTION('ref_axis',(1.,0.,0.));
#5170=DIRECTION('center_axis',(0.,1.,0.));
#5171=DIRECTION('ref_axis',(1.,0.,0.));
#5172=DIRECTION('',(0.,1.,0.));
#5173=DIRECTION('center_axis',(0.,-1.,0.));
#5174=DIRECTION('ref_axis',(1.,0.,0.));
#5175=DIRECTION('center_axis',(0.,1.,0.));
#5176=DIRECTION('ref_axis',(1.,0.,0.));
#5177=DIRECTION('center_axis',(0.,1.,0.));
#5178=DIRECTION('ref_axis',(1.,0.,0.));
#5179=DIRECTION('',(0.,1.,0.));
#5180=DIRECTION('center_axis',(0.,-1.,0.));
#5181=DIRECTION('ref_axis',(1.,0.,0.));
#5182=DIRECTION('center_axis',(0.,1.,0.));
#5183=DIRECTION('ref_axis',(1.,0.,0.));
#5184=DIRECTION('center_axis',(0.,1.,0.));
#5185=DIRECTION('ref_axis',(1.,0.,0.));
#5186=DIRECTION('',(0.,1.,0.));
#5187=DIRECTION('center_axis',(0.,-1.,0.));
#5188=DIRECTION('ref_axis',(1.,0.,0.));
#5189=DIRECTION('center_axis',(0.,1.,0.));
#5190=DIRECTION('ref_axis',(1.,0.,0.));
#5191=DIRECTION('center_axis',(0.,1.,0.));
#5192=DIRECTION('ref_axis',(1.,0.,0.));
#5193=DIRECTION('',(0.,1.,0.));
#5194=DIRECTION('center_axis',(0.,-1.,0.));
#5195=DIRECTION('ref_axis',(1.,0.,0.));
#5196=DIRECTION('center_axis',(0.,1.,0.));
#5197=DIRECTION('ref_axis',(1.,0.,0.));
#5198=DIRECTION('center_axis',(0.,1.,0.));
#5199=DIRECTION('ref_axis',(1.,0.,0.));
#5200=DIRECTION('',(0.,-1.,0.));
#5201=DIRECTION('center_axis',(0.,-1.,0.));
#5202=DIRECTION('ref_axis',(1.,0.,0.));
#5203=DIRECTION('center_axis',(0.,1.,0.));
#5204=DIRECTION('ref_axis',(1.,0.,0.));
#5205=DIRECTION('center_axis',(0.,-1.,0.));
#5206=DIRECTION('ref_axis',(1.,0.,0.));
#5207=DIRECTION('center_axis',(0.,1.,0.));
#5208=DIRECTION('ref_axis',(1.,0.,0.));
#5209=DIRECTION('center_axis',(0.,1.,0.));
#5210=DIRECTION('ref_axis',(1.,0.,0.));
#5211=DIRECTION('',(0.,1.,0.));
#5212=DIRECTION('center_axis',(0.,1.,0.));
#5213=DIRECTION('ref_axis',(1.,0.,0.));
#5214=DIRECTION('center_axis',(0.,1.,0.));
#5215=DIRECTION('ref_axis',(1.,0.,0.));
#5216=DIRECTION('center_axis',(0.,-1.,0.));
#5217=DIRECTION('ref_axis',(1.,0.,0.));
#5218=DIRECTION('center_axis',(0.,1.,0.));
#5219=DIRECTION('ref_axis',(1.,0.,0.));
#5220=DIRECTION('',(0.,-1.,0.));
#5221=DIRECTION('center_axis',(0.,1.,0.));
#5222=DIRECTION('ref_axis',(1.,0.,0.));
#5223=DIRECTION('center_axis',(0.,1.,0.));
#5224=DIRECTION('ref_axis',(1.,0.,0.));
#5225=DIRECTION('',(0.,-1.,0.));
#5226=DIRECTION('center_axis',(0.,1.,0.));
#5227=DIRECTION('ref_axis',(1.,0.,0.));
#5228=DIRECTION('center_axis',(0.,1.,0.));
#5229=DIRECTION('ref_axis',(1.,0.,0.));
#5230=DIRECTION('center_axis',(0.,1.,0.));
#5231=DIRECTION('ref_axis',(1.,0.,0.));
#5232=DIRECTION('axis',(0.,0.,1.));
#5233=DIRECTION('refdir',(1.,0.,0.));
#5234=DIRECTION('center_axis',(0.,1.,0.));
#5235=DIRECTION('ref_axis',(1.,0.,0.));
#5236=DIRECTION('center_axis',(0.,-1.,0.));
#5237=DIRECTION('ref_axis',(1.,0.,0.));
#5238=DIRECTION('',(0.,-1.,0.));
#5239=DIRECTION('center_axis',(0.,-1.,0.));
#5240=DIRECTION('ref_axis',(1.,0.,0.));
#5241=DIRECTION('center_axis',(0.,1.,0.));
#5242=DIRECTION('ref_axis',(1.,0.,0.));
#5243=DIRECTION('center_axis',(0.,1.,0.));
#5244=DIRECTION('ref_axis',(1.,0.,0.));
#5245=DIRECTION('',(0.,-1.,0.));
#5246=DIRECTION('center_axis',(0.,1.,0.));
#5247=DIRECTION('ref_axis',(1.,0.,0.));
#5248=DIRECTION('center_axis',(0.,1.,0.));
#5249=DIRECTION('ref_axis',(1.,0.,0.));
#5250=DIRECTION('center_axis',(0.,1.,0.));
#5251=DIRECTION('ref_axis',(1.,0.,0.));
#5252=DIRECTION('axis',(0.,0.,1.));
#5253=DIRECTION('refdir',(1.,0.,0.));
#5254=DIRECTION('center_axis',(0.,1.,0.));
#5255=DIRECTION('ref_axis',(1.,0.,0.));
#5256=DIRECTION('center_axis',(0.,1.,0.));
#5257=DIRECTION('ref_axis',(1.,0.,0.));
#5258=DIRECTION('',(0.,1.,0.));
#5259=DIRECTION('center_axis',(0.,-1.,0.));
#5260=DIRECTION('ref_axis',(1.,0.,0.));
#5261=DIRECTION('center_axis',(0.,1.,0.));
#5262=DIRECTION('ref_axis',(1.,0.,0.));
#5263=DIRECTION('center_axis',(0.,1.,0.));
#5264=DIRECTION('ref_axis',(1.,0.,0.));
#5265=DIRECTION('center_axis',(0.,1.,0.));
#5266=DIRECTION('ref_axis',(1.,0.,0.));
#5267=DIRECTION('center_axis',(0.,1.,0.));
#5268=DIRECTION('ref_axis',(1.,0.,0.));
#5269=DIRECTION('',(0.,1.,0.));
#5270=DIRECTION('center_axis',(0.,-1.,0.));
#5271=DIRECTION('ref_axis',(1.,0.,0.));
#5272=DIRECTION('center_axis',(0.,1.,0.));
#5273=DIRECTION('ref_axis',(1.,0.,0.));
#5274=DIRECTION('center_axis',(0.,1.,0.));
#5275=DIRECTION('ref_axis',(1.,0.,0.));
#5276=DIRECTION('center_axis',(0.,1.,0.));
#5277=DIRECTION('ref_axis',(1.,0.,0.));
#5278=DIRECTION('center_axis',(0.,1.,0.));
#5279=DIRECTION('ref_axis',(1.,0.,0.));
#5280=DIRECTION('',(0.,1.,0.));
#5281=DIRECTION('center_axis',(0.,-1.,0.));
#5282=DIRECTION('ref_axis',(1.,0.,0.));
#5283=DIRECTION('center_axis',(0.,1.,0.));
#5284=DIRECTION('ref_axis',(1.,0.,0.));
#5285=DIRECTION('center_axis',(0.,1.,0.));
#5286=DIRECTION('ref_axis',(1.,0.,0.));
#5287=DIRECTION('center_axis',(0.,1.,0.));
#5288=DIRECTION('ref_axis',(1.,0.,0.));
#5289=DIRECTION('center_axis',(0.,1.,0.));
#5290=DIRECTION('ref_axis',(1.,0.,0.));
#5291=DIRECTION('',(0.,1.,0.));
#5292=DIRECTION('center_axis',(0.,-1.,0.));
#5293=DIRECTION('ref_axis',(1.,0.,0.));
#5294=DIRECTION('center_axis',(0.,1.,0.));
#5295=DIRECTION('ref_axis',(1.,0.,0.));
#5296=DIRECTION('center_axis',(0.,1.,0.));
#5297=DIRECTION('ref_axis',(1.,0.,0.));
#5298=DIRECTION('center_axis',(0.,1.,0.));
#5299=DIRECTION('ref_axis',(1.,0.,0.));
#5300=DIRECTION('center_axis',(0.,1.,0.));
#5301=DIRECTION('ref_axis',(1.,0.,0.));
#5302=DIRECTION('',(0.,1.,0.));
#5303=DIRECTION('center_axis',(0.,1.,0.));
#5304=DIRECTION('ref_axis',(1.,0.,0.));
#5305=DIRECTION('center_axis',(0.,1.,0.));
#5306=DIRECTION('ref_axis',(1.,0.,0.));
#5307=DIRECTION('',(0.,1.,0.));
#5308=DIRECTION('center_axis',(0.,1.,0.));
#5309=DIRECTION('ref_axis',(1.,0.,0.));
#5310=DIRECTION('center_axis',(0.,1.,0.));
#5311=DIRECTION('ref_axis',(1.,0.,0.));
#5312=DIRECTION('',(0.,1.,0.));
#5313=DIRECTION('center_axis',(0.,1.,0.));
#5314=DIRECTION('ref_axis',(1.,0.,0.));
#5315=DIRECTION('center_axis',(0.,1.,0.));
#5316=DIRECTION('ref_axis',(1.,0.,0.));
#5317=DIRECTION('',(0.,1.,0.));
#5318=DIRECTION('center_axis',(0.,1.,0.));
#5319=DIRECTION('ref_axis',(1.,0.,0.));
#5320=DIRECTION('center_axis',(0.,1.,0.));
#5321=DIRECTION('ref_axis',(1.,0.,0.));
#5322=DIRECTION('center_axis',(0.,-1.,0.));
#5323=DIRECTION('ref_axis',(1.,0.,0.));
#5324=DIRECTION('center_axis',(0.,1.,0.));
#5325=DIRECTION('ref_axis',(1.,0.,0.));
#5326=DIRECTION('',(0.,-1.,0.));
#5327=DIRECTION('center_axis',(0.,-1.,0.));
#5328=DIRECTION('ref_axis',(1.,0.,0.));
#5329=DIRECTION('center_axis',(0.,1.,0.));
#5330=DIRECTION('ref_axis',(1.,0.,0.));
#5331=DIRECTION('center_axis',(0.,1.,0.));
#5332=DIRECTION('ref_axis',(1.,0.,0.));
#5333=DIRECTION('',(0.,-1.,0.));
#5334=DIRECTION('center_axis',(0.,1.,0.));
#5335=DIRECTION('ref_axis',(1.,0.,0.));
#5336=DIRECTION('center_axis',(0.,1.,0.));
#5337=DIRECTION('ref_axis',(1.,0.,0.));
#5338=DIRECTION('center_axis',(0.,1.,0.));
#5339=DIRECTION('ref_axis',(1.,0.,0.));
#5340=DIRECTION('',(0.,1.,0.));
#5341=DIRECTION('center_axis',(0.,1.,0.));
#5342=DIRECTION('ref_axis',(1.,0.,0.));
#5343=DIRECTION('center_axis',(0.,1.,0.));
#5344=DIRECTION('ref_axis',(1.,0.,0.));
#5345=DIRECTION('center_axis',(0.,1.,0.));
#5346=DIRECTION('ref_axis',(1.,0.,0.));
#5347=DIRECTION('center_axis',(0.,1.,0.));
#5348=DIRECTION('ref_axis',(1.,0.,0.));
#5349=DIRECTION('',(0.,-1.,0.));
#5350=DIRECTION('center_axis',(0.,1.,0.));
#5351=DIRECTION('ref_axis',(1.,0.,0.));
#5352=DIRECTION('center_axis',(0.,1.,0.));
#5353=DIRECTION('ref_axis',(1.,0.,0.));
#5354=DIRECTION('center_axis',(0.,1.,0.));
#5355=DIRECTION('ref_axis',(1.,0.,0.));
#5356=DIRECTION('axis',(0.,0.,1.));
#5357=DIRECTION('refdir',(1.,0.,0.));
#5358=DIRECTION('center_axis',(0.,1.,0.));
#5359=DIRECTION('ref_axis',(-1.,0.,0.));
#5360=DIRECTION('',(-1.,0.,0.));
#5361=DIRECTION('',(0.,0.,1.));
#5362=DIRECTION('',(-1.,0.,0.));
#5363=DIRECTION('',(0.,0.,1.));
#5364=DIRECTION('center_axis',(1.,0.,0.));
#5365=DIRECTION('ref_axis',(0.,1.,0.));
#5366=DIRECTION('',(0.,1.,0.));
#5367=DIRECTION('',(0.,1.,0.));
#5368=DIRECTION('',(0.,0.,1.));
#5369=DIRECTION('center_axis',(0.,-1.,0.));
#5370=DIRECTION('ref_axis',(1.,0.,0.));
#5371=DIRECTION('',(1.,0.,0.));
#5372=DIRECTION('',(1.,0.,0.));
#5373=DIRECTION('',(0.,0.,1.));
#5374=DIRECTION('center_axis',(-1.,0.,0.));
#5375=DIRECTION('ref_axis',(0.,-1.,0.));
#5376=DIRECTION('',(0.,-1.,0.));
#5377=DIRECTION('',(0.,-1.,0.));
#5378=DIRECTION('center_axis',(0.,0.,1.));
#5379=DIRECTION('ref_axis',(1.,0.,0.));
#5380=DIRECTION('center_axis',(0.,0.,1.));
#5381=DIRECTION('ref_axis',(1.,0.,0.));
#5382=DIRECTION('axis',(0.,0.,1.));
#5383=DIRECTION('refdir',(1.,0.,0.));
#5384=DIRECTION('center_axis',(0.,1.,0.));
#5385=DIRECTION('ref_axis',(-1.,0.,0.));
#5386=DIRECTION('',(-1.,0.,0.));
#5387=DIRECTION('',(0.,0.,1.));
#5388=DIRECTION('',(-1.,0.,0.));
#5389=DIRECTION('',(0.,0.,1.));
#5390=DIRECTION('center_axis',(1.,0.,0.));
#5391=DIRECTION('ref_axis',(0.,1.,0.));
#5392=DIRECTION('',(0.,1.,0.));
#5393=DIRECTION('',(0.,1.,0.));
#5394=DIRECTION('',(0.,0.,1.));
#5395=DIRECTION('center_axis',(0.,-1.,0.));
#5396=DIRECTION('ref_axis',(1.,0.,0.));
#5397=DIRECTION('',(1.,0.,0.));
#5398=DIRECTION('',(1.,0.,0.));
#5399=DIRECTION('',(0.,0.,1.));
#5400=DIRECTION('center_axis',(-1.,0.,0.));
#5401=DIRECTION('ref_axis',(0.,-1.,0.));
#5402=DIRECTION('',(0.,-1.,0.));
#5403=DIRECTION('',(0.,-1.,0.));
#5404=DIRECTION('center_axis',(0.,0.,1.));
#5405=DIRECTION('ref_axis',(1.,0.,0.));
#5406=DIRECTION('center_axis',(0.,0.,1.));
#5407=DIRECTION('ref_axis',(1.,0.,0.));
#5408=DIRECTION('axis',(0.,0.,1.));
#5409=DIRECTION('refdir',(1.,0.,0.));
#5410=DIRECTION('axis',(0.,0.,1.));
#5411=DIRECTION('refdir',(1.,0.,0.));
#5412=DIRECTION('center_axis',(0.,-1.,0.));
#5413=DIRECTION('ref_axis',(0.,0.,-1.));
#5414=DIRECTION('center_axis',(0.,-1.,0.));
#5415=DIRECTION('ref_axis',(1.,0.,0.));
#5416=DIRECTION('center_axis',(0.,-1.,0.));
#5417=DIRECTION('ref_axis',(1.,0.,0.));
#5418=DIRECTION('center_axis',(1.,0.,1.22464679914735E-16));
#5419=DIRECTION('ref_axis',(-1.22464679914735E-16,0.,1.));
#5420=DIRECTION('center_axis',(0.,1.,0.));
#5421=DIRECTION('ref_axis',(1.,0.,0.));
#5422=DIRECTION('center_axis',(0.,1.,0.));
#5423=DIRECTION('ref_axis',(1.,0.,0.));
#5424=DIRECTION('center_axis',(0.,-1.,0.));
#5425=DIRECTION('ref_axis',(1.,0.,0.));
#5426=DIRECTION('',(0.,1.,0.));
#5427=DIRECTION('center_axis',(0.,-1.,0.));
#5428=DIRECTION('ref_axis',(1.,0.,0.));
#5429=DIRECTION('center_axis',(0.,-1.,0.));
#5430=DIRECTION('ref_axis',(1.,0.,0.));
#5431=DIRECTION('center_axis',(0.,-1.,0.));
#5432=DIRECTION('ref_axis',(1.,0.,0.));
#5433=DIRECTION('',(0.,1.,0.));
#5434=DIRECTION('center_axis',(0.,-1.,0.));
#5435=DIRECTION('ref_axis',(1.,0.,0.));
#5436=DIRECTION('center_axis',(0.,1.,0.));
#5437=DIRECTION('ref_axis',(1.,0.,0.));
#5438=DIRECTION('',(-0.707106781186548,0.707106781186547,-8.65956056235494E-17));
#5439=DIRECTION('center_axis',(0.,-1.,0.));
#5440=DIRECTION('ref_axis',(1.,0.,0.));
#5441=DIRECTION('center_axis',(0.,1.,0.));
#5442=DIRECTION('ref_axis',(0.,0.,1.));
#5443=DIRECTION('center_axis',(0.,-1.,0.));
#5444=DIRECTION('ref_axis',(1.,0.,0.));
#5445=DIRECTION('center_axis',(0.,-1.,0.));
#5446=DIRECTION('ref_axis',(1.,0.,0.));
#5447=DIRECTION('',(0.,1.,0.));
#5448=DIRECTION('center_axis',(0.,-1.,0.));
#5449=DIRECTION('ref_axis',(0.,0.,-1.));
#5450=DIRECTION('center_axis',(0.,-1.,0.));
#5451=DIRECTION('ref_axis',(1.,0.,0.));
#5452=DIRECTION('center_axis',(0.,-1.,0.));
#5453=DIRECTION('ref_axis',(1.,0.,0.));
#5454=DIRECTION('',(0.707106781186548,0.707106781186547,8.65956056235494E-17));
#5455=DIRECTION('axis',(0.,0.,1.));
#5456=DIRECTION('refdir',(1.,0.,0.));
#5457=DIRECTION('center_axis',(0.,-1.,0.));
#5458=DIRECTION('ref_axis',(0.,0.,-1.));
#5459=DIRECTION('center_axis',(0.,-1.,0.));
#5460=DIRECTION('ref_axis',(1.,0.,0.));
#5461=DIRECTION('center_axis',(0.,-1.,0.));
#5462=DIRECTION('ref_axis',(1.,0.,0.));
#5463=DIRECTION('center_axis',(1.,0.,1.22464679914735E-16));
#5464=DIRECTION('ref_axis',(-1.22464679914735E-16,0.,1.));
#5465=DIRECTION('center_axis',(0.,1.,0.));
#5466=DIRECTION('ref_axis',(1.,0.,0.));
#5467=DIRECTION('center_axis',(0.,1.,0.));
#5468=DIRECTION('ref_axis',(1.,0.,0.));
#5469=DIRECTION('center_axis',(0.,-1.,0.));
#5470=DIRECTION('ref_axis',(1.,0.,0.));
#5471=DIRECTION('center_axis',(0.,-1.,0.));
#5472=DIRECTION('ref_axis',(1.,0.,0.));
#5473=DIRECTION('',(0.,1.,0.));
#5474=DIRECTION('center_axis',(0.,1.,0.));
#5475=DIRECTION('ref_axis',(0.,0.,1.));
#5476=DIRECTION('center_axis',(0.,-1.,0.));
#5477=DIRECTION('ref_axis',(1.,0.,0.));
#5478=DIRECTION('center_axis',(0.,-1.,0.));
#5479=DIRECTION('ref_axis',(1.,0.,0.));
#5480=DIRECTION('center_axis',(0.,-1.,0.));
#5481=DIRECTION('ref_axis',(1.,0.,0.));
#5482=DIRECTION('center_axis',(0.,-1.,0.));
#5483=DIRECTION('ref_axis',(1.,0.,0.));
#5484=DIRECTION('',(0.707106781186548,0.707106781186547,8.65956056235494E-17));
#5485=DIRECTION('center_axis',(0.,-1.,0.));
#5486=DIRECTION('ref_axis',(1.,0.,0.));
#5487=DIRECTION('center_axis',(0.,-1.,0.));
#5488=DIRECTION('ref_axis',(1.,0.,0.));
#5489=DIRECTION('',(0.,1.,0.));
#5490=DIRECTION('center_axis',(0.,1.,0.));
#5491=DIRECTION('ref_axis',(1.,0.,0.));
#5492=DIRECTION('center_axis',(0.,-1.,0.));
#5493=DIRECTION('ref_axis',(1.,0.,0.));
#5494=DIRECTION('',(-0.707106781186548,0.707106781186547,-8.65956056235494E-17));
#5495=DIRECTION('center_axis',(0.,-1.,0.));
#5496=DIRECTION('ref_axis',(0.,0.,-1.));
#5497=DIRECTION('center_axis',(0.,-1.,0.));
#5498=DIRECTION('ref_axis',(1.,0.,0.));
#5499=DIRECTION('',(0.,1.,0.));
#5500=DIRECTION('axis',(0.,0.,1.));
#5501=DIRECTION('refdir',(1.,0.,0.));
#5502=DIRECTION('center_axis',(0.,0.,1.));
#5503=DIRECTION('ref_axis',(1.,0.,0.));
#5504=DIRECTION('center_axis',(1.22464679914735E-16,-1.,0.));
#5505=DIRECTION('ref_axis',(-1.,-1.22464679914735E-16,0.));
#5506=DIRECTION('center_axis',(0.707106781186548,0.,0.707106781186548));
#5507=DIRECTION('ref_axis',(0.707106781186548,0.,-0.707106781186548));
#5508=DIRECTION('center_axis',(8.65956056235493E-17,-1.,-8.65956056235493E-17));
#5509=DIRECTION('ref_axis',(-0.707106781186548,-1.22464679914735E-16,0.707106781186548));
#5510=DIRECTION('center_axis',(1.,0.,0.));
#5511=DIRECTION('ref_axis',(6.12323399573677E-17,0.,-1.));
#5512=DIRECTION('center_axis',(7.49879891330929E-33,-1.,-1.22464679914735E-16));
#5513=DIRECTION('ref_axis',(-6.12323399573677E-17,-1.22464679914735E-16,
1.));
#5514=DIRECTION('center_axis',(0.707106781186548,0.,-0.707106781186548));
#5515=DIRECTION('ref_axis',(-0.707106781186548,0.,-0.707106781186548));
#5516=DIRECTION('center_axis',(-8.65956056235493E-17,-1.,-8.65956056235493E-17));
#5517=DIRECTION('ref_axis',(0.707106781186548,-1.22464679914735E-16,0.707106781186548));
#5518=DIRECTION('center_axis',(0.,0.,-1.));
#5519=DIRECTION('ref_axis',(-1.,0.,-1.22464679914735E-16));
#5520=DIRECTION('center_axis',(-1.22464679914735E-16,-1.,-1.49975978266186E-32));
#5521=DIRECTION('ref_axis',(1.,-1.22464679914735E-16,1.22464679914735E-16));
#5522=DIRECTION('center_axis',(-0.707106781186548,0.,-0.707106781186548));
#5523=DIRECTION('ref_axis',(-0.707106781186548,0.,0.707106781186548));
#5524=DIRECTION('center_axis',(-8.65956056235493E-17,-1.,8.65956056235493E-17));
#5525=DIRECTION('ref_axis',(0.707106781186548,-1.22464679914735E-16,-0.707106781186548));
#5526=DIRECTION('center_axis',(-1.,0.,0.));
#5527=DIRECTION('ref_axis',(-1.83697019872103E-16,0.,1.));
#5528=DIRECTION('center_axis',(-2.24963967399279E-32,-1.,1.22464679914735E-16));
#5529=DIRECTION('ref_axis',(1.83697019872103E-16,-1.22464679914735E-16,
-1.));
#5530=DIRECTION('center_axis',(-0.707106781186548,0.,0.707106781186548));
#5531=DIRECTION('ref_axis',(0.707106781186548,0.,0.707106781186548));
#5532=DIRECTION('center_axis',(8.65956056235493E-17,-1.,8.65956056235494E-17));
#5533=DIRECTION('ref_axis',(-0.707106781186548,-1.22464679914735E-16,-0.707106781186548));
#5534=DIRECTION('axis',(0.,0.,1.));
#5535=DIRECTION('refdir',(1.,0.,0.));
#5536=DIRECTION('center_axis',(0.,0.,1.));
#5537=DIRECTION('ref_axis',(1.,0.,0.));
#5538=DIRECTION('center_axis',(0.,-1.,0.));
#5539=DIRECTION('ref_axis',(0.,0.,-1.));
#5540=DIRECTION('center_axis',(0.,-1.,0.));
#5541=DIRECTION('ref_axis',(0.,0.,-1.));
#5542=DIRECTION('center_axis',(0.,1.,0.));
#5543=DIRECTION('ref_axis',(1.,0.,0.));
#5544=DIRECTION('center_axis',(0.,1.,0.));
#5545=DIRECTION('ref_axis',(1.,0.,0.));
#5546=DIRECTION('center_axis',(0.,1.,0.));
#5547=DIRECTION('ref_axis',(1.,0.,0.));
#5548=DIRECTION('center_axis',(0.,1.,0.));
#5549=DIRECTION('ref_axis',(1.,0.,0.));
#5550=DIRECTION('',(0.,-1.,0.));
#5551=DIRECTION('center_axis',(0.,-1.,0.));
#5552=DIRECTION('ref_axis',(1.,0.,0.));
#5553=DIRECTION('center_axis',(0.,1.,0.));
#5554=DIRECTION('ref_axis',(1.,0.,0.));
#5555=DIRECTION('center_axis',(0.,1.,0.));
#5556=DIRECTION('ref_axis',(1.,0.,0.));
#5557=DIRECTION('center_axis',(0.,1.,0.));
#5558=DIRECTION('ref_axis',(1.,0.,0.));
#5559=DIRECTION('center_axis',(0.,1.,0.));
#5560=DIRECTION('ref_axis',(1.,0.,0.));
#5561=DIRECTION('center_axis',(0.,1.,0.));
#5562=DIRECTION('ref_axis',(1.,0.,0.));
#5563=DIRECTION('center_axis',(0.,1.,0.));
#5564=DIRECTION('ref_axis',(1.,0.,0.));
#5565=DIRECTION('center_axis',(0.,-1.,0.));
#5566=DIRECTION('ref_axis',(1.,0.,0.));
#5567=DIRECTION('center_axis',(0.,-1.,0.));
#5568=DIRECTION('ref_axis',(0.,0.,-1.));
#5569=DIRECTION('center_axis',(6.12323399573677E-17,0.,1.));
#5570=DIRECTION('ref_axis',(1.,0.,0.));
#5571=DIRECTION('center_axis',(0.,-1.,0.));
#5572=DIRECTION('ref_axis',(0.,0.,-1.));
#5573=DIRECTION('center_axis',(0.,1.,0.));
#5574=DIRECTION('ref_axis',(1.,0.,0.));
#5575=DIRECTION('center_axis',(0.,-1.,0.));
#5576=DIRECTION('ref_axis',(1.,0.,0.));
#5577=DIRECTION('center_axis',(0.,-1.,0.));
#5578=DIRECTION('ref_axis',(0.,0.,-1.));
#5579=DIRECTION('center_axis',(0.,0.,1.));
#5580=DIRECTION('ref_axis',(1.,0.,0.));
#5581=DIRECTION('center_axis',(0.,-1.,0.));
#5582=DIRECTION('ref_axis',(0.,0.,-1.));
#5583=DIRECTION('center_axis',(0.,1.,0.));
#5584=DIRECTION('ref_axis',(1.,0.,0.));
#5585=DIRECTION('center_axis',(0.,-1.,0.));
#5586=DIRECTION('ref_axis',(1.,0.,0.));
#5587=DIRECTION('center_axis',(0.,-1.,0.));
#5588=DIRECTION('ref_axis',(0.,0.,-1.));
#5589=DIRECTION('center_axis',(0.,0.,1.));
#5590=DIRECTION('ref_axis',(1.,0.,0.));
#5591=DIRECTION('center_axis',(0.,-1.,0.));
#5592=DIRECTION('ref_axis',(0.,0.,-1.));
#5593=DIRECTION('center_axis',(0.,1.,0.));
#5594=DIRECTION('ref_axis',(1.,0.,0.));
#5595=DIRECTION('center_axis',(0.,-1.,0.));
#5596=DIRECTION('ref_axis',(1.,0.,0.));
#5597=DIRECTION('center_axis',(0.,-1.,0.));
#5598=DIRECTION('ref_axis',(0.,0.,-1.));
#5599=DIRECTION('center_axis',(0.,0.,1.));
#5600=DIRECTION('ref_axis',(1.,0.,0.));
#5601=DIRECTION('center_axis',(0.,-1.,0.));
#5602=DIRECTION('ref_axis',(0.,0.,-1.));
#5603=DIRECTION('center_axis',(0.,1.,0.));
#5604=DIRECTION('ref_axis',(1.,0.,0.));
#5605=DIRECTION('center_axis',(0.,-1.,0.));
#5606=DIRECTION('ref_axis',(1.,0.,0.));
#5607=DIRECTION('center_axis',(0.,-1.,0.));
#5608=DIRECTION('ref_axis',(0.,0.,-1.));
#5609=DIRECTION('center_axis',(6.12323399573676E-17,0.,1.));
#5610=DIRECTION('ref_axis',(1.,0.,0.));
#5611=DIRECTION('center_axis',(0.,-1.,0.));
#5612=DIRECTION('ref_axis',(0.,0.,-1.));
#5613=DIRECTION('center_axis',(0.,1.,0.));
#5614=DIRECTION('ref_axis',(1.,0.,0.));
#5615=DIRECTION('center_axis',(0.,-1.,0.));
#5616=DIRECTION('ref_axis',(1.,0.,0.));
#5617=DIRECTION('center_axis',(0.,-1.,0.));
#5618=DIRECTION('ref_axis',(0.,0.,-1.));
#5619=DIRECTION('center_axis',(0.,0.,1.));
#5620=DIRECTION('ref_axis',(1.,0.,0.));
#5621=DIRECTION('center_axis',(0.,-1.,0.));
#5622=DIRECTION('ref_axis',(0.,0.,-1.));
#5623=DIRECTION('center_axis',(0.,1.,0.));
#5624=DIRECTION('ref_axis',(1.,0.,0.));
#5625=DIRECTION('center_axis',(0.,1.,0.));
#5626=DIRECTION('ref_axis',(1.,0.,0.));
#5627=DIRECTION('',(0.,1.,0.));
#5628=DIRECTION('center_axis',(0.,-1.,0.));
#5629=DIRECTION('ref_axis',(1.,0.,0.));
#5630=DIRECTION('center_axis',(0.,-1.,0.));
#5631=DIRECTION('ref_axis',(1.,0.,0.));
#5632=DIRECTION('center_axis',(0.,1.,0.));
#5633=DIRECTION('ref_axis',(1.,0.,0.));
#5634=DIRECTION('center_axis',(0.,-1.,0.));
#5635=DIRECTION('ref_axis',(0.,0.,-1.));
#5636=DIRECTION('center_axis',(0.,0.,1.));
#5637=DIRECTION('ref_axis',(1.,0.,0.));
#5638=DIRECTION('center_axis',(0.,-1.,0.));
#5639=DIRECTION('ref_axis',(0.,0.,-1.));
#5640=DIRECTION('center_axis',(0.,-1.,0.));
#5641=DIRECTION('ref_axis',(-1.,0.,0.));
#5642=DIRECTION('center_axis',(0.,1.,0.));
#5643=DIRECTION('ref_axis',(1.,0.,0.));
#5644=DIRECTION('axis',(0.,0.,1.));
#5645=DIRECTION('refdir',(1.,0.,0.));
#5646=DIRECTION('center_axis',(0.,1.,0.));
#5647=DIRECTION('ref_axis',(0.,0.,1.));
#5648=DIRECTION('center_axis',(0.,-1.,0.));
#5649=DIRECTION('ref_axis',(1.,0.,0.));
#5650=DIRECTION('center_axis',(0.,-1.,0.));
#5651=DIRECTION('ref_axis',(1.,0.,0.));
#5652=DIRECTION('center_axis',(0.,-1.,0.));
#5653=DIRECTION('ref_axis',(1.,0.,0.));
#5654=DIRECTION('center_axis',(0.,-1.,0.));
#5655=DIRECTION('ref_axis',(1.,0.,0.));
#5656=DIRECTION('',(0.,1.,0.));
#5657=DIRECTION('center_axis',(0.,-1.,0.));
#5658=DIRECTION('ref_axis',(0.,0.,-1.));
#5659=DIRECTION('center_axis',(0.,-1.,0.));
#5660=DIRECTION('ref_axis',(1.,0.,0.));
#5661=DIRECTION('center_axis',(0.,-1.,0.));
#5662=DIRECTION('ref_axis',(1.,0.,0.));
#5663=DIRECTION('',(0.,1.,0.));
#5664=DIRECTION('center_axis',(0.,1.,0.));
#5665=DIRECTION('ref_axis',(0.,0.,1.));
#5666=DIRECTION('center_axis',(0.,-1.,0.));
#5667=DIRECTION('ref_axis',(1.,0.,0.));
#5668=DIRECTION('center_axis',(0.,-1.,0.));
#5669=DIRECTION('ref_axis',(1.,0.,0.));
#5670=DIRECTION('center_axis',(0.,-1.,0.));
#5671=DIRECTION('ref_axis',(1.,0.,0.));
#5672=DIRECTION('center_axis',(0.,-1.,0.));
#5673=DIRECTION('ref_axis',(1.,0.,0.));
#5674=DIRECTION('',(0.,1.,0.));
#5675=DIRECTION('center_axis',(0.,-1.,0.));
#5676=DIRECTION('ref_axis',(0.,0.,-1.));
#5677=DIRECTION('center_axis',(0.,-1.,0.));
#5678=DIRECTION('ref_axis',(1.,0.,0.));
#5679=DIRECTION('center_axis',(0.,-1.,0.));
#5680=DIRECTION('ref_axis',(1.,0.,0.));
#5681=DIRECTION('',(0.,1.,0.));
#5682=DIRECTION('',(0.,0.,1.));
#5683=DIRECTION('',(1.,0.,0.));
#5684=DIRECTION('',(0.,0.,1.));
#5685=DIRECTION('',(1.,0.,0.));
#5686=DIRECTION('',(0.,0.,1.));
#5687=DIRECTION('',(1.,0.,0.));
#5688=DIRECTION('',(0.,0.,1.));
#5689=DIRECTION('',(1.,0.,0.));
#5690=DIRECTION('',(0.,0.,1.));
#5691=DIRECTION('',(1.,0.,0.));
#5692=DIRECTION('axis',(0.,0.,1.));
#5693=DIRECTION('refdir',(1.,0.,0.));
#5694=DIRECTION('center_axis',(0.,1.,0.));
#5695=DIRECTION('ref_axis',(0.,0.,1.));
#5696=DIRECTION('center_axis',(0.,-1.,0.));
#5697=DIRECTION('ref_axis',(1.,0.,0.));
#5698=DIRECTION('center_axis',(0.,-1.,0.));
#5699=DIRECTION('ref_axis',(1.,0.,0.));
#5700=DIRECTION('center_axis',(0.,-1.,0.));
#5701=DIRECTION('ref_axis',(1.,0.,0.));
#5702=DIRECTION('',(0.707106781186548,0.707106781186547,8.65956056235494E-17));
#5703=DIRECTION('center_axis',(0.,-1.,0.));
#5704=DIRECTION('ref_axis',(1.,0.,0.));
#5705=DIRECTION('center_axis',(0.,-1.,0.));
#5706=DIRECTION('ref_axis',(1.,0.,0.));
#5707=DIRECTION('',(0.,1.,0.));
#5708=DIRECTION('center_axis',(0.,1.,0.));
#5709=DIRECTION('ref_axis',(1.,0.,0.));
#5710=DIRECTION('center_axis',(0.,-1.,0.));
#5711=DIRECTION('ref_axis',(1.,0.,0.));
#5712=DIRECTION('',(-0.707106781186547,0.707106781186548,-8.65956056235493E-17));
#5713=DIRECTION('center_axis',(0.,-1.,0.));
#5714=DIRECTION('ref_axis',(0.,0.,-1.));
#5715=DIRECTION('center_axis',(0.,-1.,0.));
#5716=DIRECTION('ref_axis',(1.,0.,0.));
#5717=DIRECTION('center_axis',(0.,1.,0.));
#5718=DIRECTION('ref_axis',(1.,0.,0.));
#5719=DIRECTION('center_axis',(0.,1.,0.));
#5720=DIRECTION('ref_axis',(1.,0.,0.));
#5721=DIRECTION('',(-0.447213595499958,0.894427190999916,-5.47678698264203E-17));
#5722=DIRECTION('center_axis',(0.,-1.,0.));
#5723=DIRECTION('ref_axis',(1.,0.,0.));
#5724=DIRECTION('center_axis',(0.,1.,0.));
#5725=DIRECTION('ref_axis',(1.,0.,0.));
#5726=DIRECTION('',(0.,1.,0.));
#5727=DIRECTION('center_axis',(0.,1.,0.));
#5728=DIRECTION('ref_axis',(1.,0.,0.));
#5729=DIRECTION('center_axis',(0.,-1.,0.));
#5730=DIRECTION('ref_axis',(1.,0.,0.));
#5731=DIRECTION('',(-0.707106781186547,0.707106781186548,-8.65956056235493E-17));
#5732=DIRECTION('center_axis',(0.,-1.,0.));
#5733=DIRECTION('ref_axis',(0.,0.,-1.));
#5734=DIRECTION('center_axis',(0.866025403784439,0.,-0.5));
#5735=DIRECTION('ref_axis',(0.5,0.,0.866025403784439));
#5736=DIRECTION('',(-0.5,0.,-0.866025403784439));
#5737=DIRECTION('',(0.,-1.,0.));
#5738=DIRECTION('',(0.5,0.,0.866025403784439));
#5739=DIRECTION('',(0.,-1.,0.));
#5740=DIRECTION('center_axis',(1.92296268638356E-16,0.,-1.));
#5741=DIRECTION('ref_axis',(1.,0.,1.92296268638356E-16));
#5742=DIRECTION('',(-1.,0.,-1.92296268638356E-16));
#5743=DIRECTION('',(0.,-1.,0.));
#5744=DIRECTION('',(1.,0.,1.92296268638356E-16));
#5745=DIRECTION('center_axis',(-0.866025403784439,0.,-0.5));
#5746=DIRECTION('ref_axis',(0.5,0.,-0.866025403784439));
#5747=DIRECTION('',(-0.5,0.,0.866025403784438));
#5748=DIRECTION('',(0.,-1.,0.));
#5749=DIRECTION('',(0.5,0.,-0.866025403784438));
#5750=DIRECTION('center_axis',(-0.866025403784439,0.,0.5));
#5751=DIRECTION('ref_axis',(-0.5,0.,-0.866025403784439));
#5752=DIRECTION('',(0.5,0.,0.866025403784439));
#5753=DIRECTION('',(0.,-1.,0.));
#5754=DIRECTION('',(-0.5,0.,-0.866025403784439));
#5755=DIRECTION('center_axis',(-1.92296268638356E-16,0.,1.));
#5756=DIRECTION('ref_axis',(-1.,0.,-1.92296268638356E-16));
#5757=DIRECTION('',(1.,0.,1.92296268638356E-16));
#5758=DIRECTION('',(0.,-1.,0.));
#5759=DIRECTION('',(-1.,0.,-1.92296268638356E-16));
#5760=DIRECTION('center_axis',(0.866025403784439,0.,0.5));
#5761=DIRECTION('ref_axis',(-0.5,0.,0.866025403784439));
#5762=DIRECTION('',(0.5,0.,-0.866025403784439));
#5763=DIRECTION('',(-0.5,0.,0.866025403784439));
#5764=DIRECTION('center_axis',(0.,1.,0.));
#5765=DIRECTION('ref_axis',(1.,0.,0.));
#5766=DIRECTION('center_axis',(0.,-1.,0.));
#5767=DIRECTION('ref_axis',(0.,0.,-1.));
#5768=DIRECTION('axis',(0.,0.,1.));
#5769=DIRECTION('refdir',(1.,0.,0.));
#5770=DIRECTION('center_axis',(0.,1.,0.));
#5771=DIRECTION('ref_axis',(0.,0.,1.));
#5772=DIRECTION('center_axis',(0.,-1.,0.));
#5773=DIRECTION('ref_axis',(1.,0.,0.));
#5774=DIRECTION('center_axis',(0.,-1.,0.));
#5775=DIRECTION('ref_axis',(1.,0.,0.));
#5776=DIRECTION('center_axis',(0.,-1.,0.));
#5777=DIRECTION('ref_axis',(1.,0.,0.));
#5778=DIRECTION('',(0.707106781186547,0.707106781186548,8.65956056235493E-17));
#5779=DIRECTION('center_axis',(0.,-1.,0.));
#5780=DIRECTION('ref_axis',(1.,0.,0.));
#5781=DIRECTION('center_axis',(0.,-1.,0.));
#5782=DIRECTION('ref_axis',(1.,0.,0.));
#5783=DIRECTION('',(0.,1.,0.));
#5784=DIRECTION('center_axis',(0.,1.,0.));
#5785=DIRECTION('ref_axis',(1.,0.,0.));
#5786=DIRECTION('center_axis',(0.,-1.,0.));
#5787=DIRECTION('ref_axis',(1.,0.,0.));
#5788=DIRECTION('',(-0.707106781186547,0.707106781186548,-8.65956056235493E-17));
#5789=DIRECTION('center_axis',(0.,-1.,0.));
#5790=DIRECTION('ref_axis',(0.,0.,-1.));
#5791=DIRECTION('center_axis',(0.,-1.,0.));
#5792=DIRECTION('ref_axis',(1.,0.,0.));
#5793=DIRECTION('center_axis',(0.,1.,0.));
#5794=DIRECTION('ref_axis',(1.,0.,0.));
#5795=DIRECTION('center_axis',(0.,1.,0.));
#5796=DIRECTION('ref_axis',(1.,0.,0.));
#5797=DIRECTION('',(-0.447213595499958,0.894427190999916,-5.47678698264203E-17));
#5798=DIRECTION('center_axis',(0.,-1.,0.));
#5799=DIRECTION('ref_axis',(1.,0.,0.));
#5800=DIRECTION('center_axis',(0.,1.,0.));
#5801=DIRECTION('ref_axis',(1.,0.,0.));
#5802=DIRECTION('',(0.,1.,0.));
#5803=DIRECTION('center_axis',(0.,1.,0.));
#5804=DIRECTION('ref_axis',(1.,0.,0.));
#5805=DIRECTION('center_axis',(0.,-1.,0.));
#5806=DIRECTION('ref_axis',(1.,0.,0.));
#5807=DIRECTION('',(-0.707106781186547,0.707106781186548,-8.65956056235493E-17));
#5808=DIRECTION('center_axis',(0.,-1.,0.));
#5809=DIRECTION('ref_axis',(0.,0.,-1.));
#5810=DIRECTION('center_axis',(0.866025403784439,0.,-0.5));
#5811=DIRECTION('ref_axis',(0.5,0.,0.866025403784439));
#5812=DIRECTION('',(-0.5,0.,-0.866025403784439));
#5813=DIRECTION('',(0.,-1.,0.));
#5814=DIRECTION('',(0.5,0.,0.866025403784439));
#5815=DIRECTION('',(0.,-1.,0.));
#5816=DIRECTION('center_axis',(1.60246890531964E-16,0.,-1.));
#5817=DIRECTION('ref_axis',(1.,0.,1.60246890531964E-16));
#5818=DIRECTION('',(-1.,0.,-1.60246890531964E-16));
#5819=DIRECTION('',(0.,-1.,0.));
#5820=DIRECTION('',(1.,0.,1.60246890531964E-16));
#5821=DIRECTION('center_axis',(-0.866025403784439,0.,-0.5));
#5822=DIRECTION('ref_axis',(0.5,0.,-0.866025403784439));
#5823=DIRECTION('',(-0.5,0.,0.866025403784439));
#5824=DIRECTION('',(0.,-1.,0.));
#5825=DIRECTION('',(0.5,0.,-0.866025403784439));
#5826=DIRECTION('center_axis',(-0.866025403784439,0.,0.5));
#5827=DIRECTION('ref_axis',(-0.5,0.,-0.866025403784439));
#5828=DIRECTION('',(0.5,0.,0.866025403784439));
#5829=DIRECTION('',(0.,-1.,0.));
#5830=DIRECTION('',(-0.5,0.,-0.866025403784439));
#5831=DIRECTION('center_axis',(-1.60246890531964E-16,0.,1.));
#5832=DIRECTION('ref_axis',(-1.,0.,-1.60246890531964E-16));
#5833=DIRECTION('',(1.,0.,1.60246890531964E-16));
#5834=DIRECTION('',(0.,-1.,0.));
#5835=DIRECTION('',(-1.,0.,-1.60246890531964E-16));
#5836=DIRECTION('center_axis',(0.866025403784439,0.,0.5));
#5837=DIRECTION('ref_axis',(-0.5,0.,0.866025403784439));
#5838=DIRECTION('',(0.5,0.,-0.866025403784439));
#5839=DIRECTION('',(-0.5,0.,0.866025403784439));
#5840=DIRECTION('center_axis',(0.,1.,0.));
#5841=DIRECTION('ref_axis',(1.,0.,0.));
#5842=DIRECTION('center_axis',(0.,-1.,0.));
#5843=DIRECTION('ref_axis',(0.,0.,-1.));
#5844=DIRECTION('',(0.,0.,1.));
#5845=DIRECTION('',(1.,0.,0.));
#5846=DIRECTION('',(0.,0.,1.));
#5847=DIRECTION('',(1.,0.,0.));
#5848=DIRECTION('',(0.,0.,1.));
#5849=DIRECTION('',(1.,0.,0.));
#5850=DIRECTION('',(0.,0.,1.));
#5851=DIRECTION('',(1.,0.,0.));
#5852=DIRECTION('',(0.,0.,1.));
#5853=DIRECTION('',(1.,0.,0.));
#5854=DIRECTION('',(0.,0.,1.));
#5855=DIRECTION('',(1.,0.,0.));
#5856=DIRECTION('',(0.,0.,1.));
#5857=DIRECTION('',(1.,0.,0.));
#5858=DIRECTION('',(0.,0.,1.));
#5859=DIRECTION('',(1.,0.,0.));
#5860=DIRECTION('',(0.,0.,1.));
#5861=DIRECTION('',(1.,0.,0.));
#5862=DIRECTION('',(0.,-1.,2.22044604925031E-16));
#5863=DIRECTION('',(1.,0.,0.));
#5864=DIRECTION('',(0.,-1.,2.22044604925031E-16));
#5865=DIRECTION('',(1.,0.,0.));
#5866=DIRECTION('',(0.,0.,1.));
#5867=DIRECTION('',(1.,0.,0.));
#5868=DIRECTION('',(0.,-1.,2.22044604925031E-16));
#5869=DIRECTION('',(1.,0.,0.));
#5870=DIRECTION('',(0.,-1.,2.22044604925031E-16));
#5871=DIRECTION('',(1.,0.,0.));
#5872=DIRECTION('',(0.,0.,1.));
#5873=DIRECTION('',(-1.,1.22464679914735E-16,0.));
#5874=DIRECTION('',(0.,0.,1.));
#5875=DIRECTION('',(-1.,1.22464679914735E-16,0.));
#5876=DIRECTION('',(0.,0.,1.));
#5877=DIRECTION('',(-1.,1.22464679914735E-16,0.));
#5878=DIRECTION('',(0.,0.,1.));
#5879=DIRECTION('',(-1.,1.22464679914735E-16,0.));
#5880=DIRECTION('',(0.,0.,1.));
#5881=DIRECTION('',(1.,0.,0.));
#5882=DIRECTION('',(0.,0.,1.));
#5883=DIRECTION('',(1.,0.,0.));
#5884=DIRECTION('',(0.,0.,1.));
#5885=DIRECTION('',(1.,0.,0.));
#5886=DIRECTION('',(0.,0.,1.));
#5887=DIRECTION('',(1.,0.,0.));
#5888=DIRECTION('axis',(0.,0.,1.));
#5889=DIRECTION('refdir',(1.,0.,0.));
#5890=DIRECTION('axis',(0.,0.,1.));
#5891=DIRECTION('refdir',(1.,0.,0.));
#5892=DIRECTION('center_axis',(-1.,0.,0.));
#5893=DIRECTION('ref_axis',(0.,0.,1.));
#5894=DIRECTION('',(0.,-1.,0.));
#5895=DIRECTION('',(0.,0.,1.));
#5896=DIRECTION('',(0.,1.,0.));
#5897=DIRECTION('',(0.,0.,-1.));
#5898=DIRECTION('center_axis',(0.,1.,0.));
#5899=DIRECTION('ref_axis',(1.,0.,0.));
#5900=DIRECTION('center_axis',(0.,-1.,0.));
#5901=DIRECTION('ref_axis',(1.,0.,0.));
#5902=DIRECTION('',(-1.,0.,0.));
#5903=DIRECTION('',(0.,0.,1.));
#5904=DIRECTION('center_axis',(1.,0.,0.));
#5905=DIRECTION('ref_axis',(0.,0.,-1.));
#5906=DIRECTION('',(0.,1.,0.));
#5907=DIRECTION('',(0.,1.,0.));
#5908=DIRECTION('',(0.,0.,-1.));
#5909=DIRECTION('center_axis',(0.,0.,1.));
#5910=DIRECTION('ref_axis',(1.,0.,0.));
#5911=DIRECTION('',(1.,0.,0.));
#5912=DIRECTION('center_axis',(0.,1.,0.));
#5913=DIRECTION('ref_axis',(0.,0.,1.));
#5914=DIRECTION('center_axis',(0.,1.,0.));
#5915=DIRECTION('ref_axis',(1.,0.,0.));
#5916=DIRECTION('center_axis',(0.,1.,0.));
#5917=DIRECTION('ref_axis',(1.,0.,0.));
#5918=DIRECTION('center_axis',(0.,1.,0.));
#5919=DIRECTION('ref_axis',(1.,0.,0.));
#5920=DIRECTION('center_axis',(0.,1.,0.));
#5921=DIRECTION('ref_axis',(1.,0.,0.));
#5922=DIRECTION('center_axis',(0.,1.,0.));
#5923=DIRECTION('ref_axis',(1.,0.,0.));
#5924=DIRECTION('center_axis',(0.,1.,0.));
#5925=DIRECTION('ref_axis',(1.,0.,0.));
#5926=DIRECTION('center_axis',(0.,-1.,0.));
#5927=DIRECTION('ref_axis',(1.,0.,0.));
#5928=DIRECTION('center_axis',(0.,1.,0.));
#5929=DIRECTION('ref_axis',(1.,0.,0.));
#5930=DIRECTION('',(0.,-1.,0.));
#5931=DIRECTION('center_axis',(0.,1.,0.));
#5932=DIRECTION('ref_axis',(1.,0.,0.));
#5933=DIRECTION('',(0.,-1.,0.));
#5934=DIRECTION('center_axis',(0.,1.,0.));
#5935=DIRECTION('ref_axis',(1.,0.,0.));
#5936=DIRECTION('center_axis',(0.,1.,0.));
#5937=DIRECTION('ref_axis',(1.,0.,0.));
#5938=DIRECTION('center_axis',(0.,1.,0.));
#5939=DIRECTION('ref_axis',(1.,0.,0.));
#5940=DIRECTION('',(0.,-1.,0.));
#5941=DIRECTION('center_axis',(0.,1.,0.));
#5942=DIRECTION('ref_axis',(1.,0.,0.));
#5943=DIRECTION('center_axis',(0.,1.,0.));
#5944=DIRECTION('ref_axis',(1.,0.,0.));
#5945=DIRECTION('axis',(0.,0.,1.));
#5946=DIRECTION('refdir',(1.,0.,0.));
#5947=DIRECTION('center_axis',(0.,1.,0.));
#5948=DIRECTION('ref_axis',(1.,0.,0.));
#5949=DIRECTION('center_axis',(0.,-1.,0.));
#5950=DIRECTION('ref_axis',(1.,0.,0.));
#5951=DIRECTION('',(0.,-1.,0.));
#5952=DIRECTION('center_axis',(0.,-1.,0.));
#5953=DIRECTION('ref_axis',(1.,0.,0.));
#5954=DIRECTION('center_axis',(0.,1.,0.));
#5955=DIRECTION('ref_axis',(1.,0.,0.));
#5956=DIRECTION('center_axis',(0.,1.,0.));
#5957=DIRECTION('ref_axis',(1.,0.,0.));
#5958=DIRECTION('',(0.,-1.,0.));
#5959=DIRECTION('center_axis',(0.,1.,0.));
#5960=DIRECTION('ref_axis',(1.,0.,0.));
#5961=DIRECTION('center_axis',(0.,1.,0.));
#5962=DIRECTION('ref_axis',(1.,0.,0.));
#5963=DIRECTION('center_axis',(0.,1.,0.));
#5964=DIRECTION('ref_axis',(1.,0.,0.));
#5965=DIRECTION('axis',(0.,0.,1.));
#5966=DIRECTION('refdir',(1.,0.,0.));
#5967=DIRECTION('center_axis',(0.,0.,1.));
#5968=DIRECTION('ref_axis',(1.,0.,0.));
#5969=DIRECTION('',(0.,1.,0.));
#5970=DIRECTION('center_axis',(0.,0.,1.));
#5971=DIRECTION('ref_axis',(1.,0.,0.));
#5972=DIRECTION('center_axis',(0.,0.,1.));
#5973=DIRECTION('ref_axis',(1.,0.,0.));
#5974=DIRECTION('center_axis',(0.,0.,1.));
#5975=DIRECTION('ref_axis',(1.,0.,0.));
#5976=DIRECTION('',(0.,0.,1.));
#5977=DIRECTION('center_axis',(0.,0.,1.));
#5978=DIRECTION('ref_axis',(1.,0.,0.));
#5979=DIRECTION('center_axis',(0.,0.,1.));
#5980=DIRECTION('ref_axis',(1.,0.,0.));
#5981=DIRECTION('',(0.,-1.,0.));
#5982=DIRECTION('center_axis',(0.,1.,0.));
#5983=DIRECTION('ref_axis',(1.,0.,0.));
#5984=DIRECTION('center_axis',(0.,-1.,0.));
#5985=DIRECTION('ref_axis',(1.,0.,0.));
#5986=DIRECTION('',(0.,-1.,0.));
#5987=DIRECTION('center_axis',(0.,-1.,0.));
#5988=DIRECTION('ref_axis',(1.,0.,0.));
#5989=DIRECTION('center_axis',(0.,1.,0.));
#5990=DIRECTION('ref_axis',(1.,0.,0.));
#5991=DIRECTION('center_axis',(0.,1.,0.));
#5992=DIRECTION('ref_axis',(1.,0.,0.));
#5993=DIRECTION('',(0.,-1.,0.));
#5994=DIRECTION('center_axis',(0.,1.,0.));
#5995=DIRECTION('ref_axis',(1.,0.,0.));
#5996=DIRECTION('center_axis',(0.,1.,0.));
#5997=DIRECTION('ref_axis',(1.,0.,0.));
#5998=DIRECTION('center_axis',(0.,1.,0.));
#5999=DIRECTION('ref_axis',(1.,0.,0.));
#6000=DIRECTION('axis',(0.,0.,1.));
#6001=DIRECTION('refdir',(1.,0.,0.));
#6002=DIRECTION('center_axis',(0.,0.,1.));
#6003=DIRECTION('ref_axis',(1.,0.,0.));
#6004=DIRECTION('',(0.,1.,0.));
#6005=DIRECTION('center_axis',(0.,0.,1.));
#6006=DIRECTION('ref_axis',(1.,0.,0.));
#6007=DIRECTION('center_axis',(0.,0.,1.));
#6008=DIRECTION('ref_axis',(1.,0.,0.));
#6009=DIRECTION('center_axis',(0.,0.,1.));
#6010=DIRECTION('ref_axis',(1.,0.,0.));
#6011=DIRECTION('',(0.,0.,1.));
#6012=DIRECTION('center_axis',(0.,0.,1.));
#6013=DIRECTION('ref_axis',(1.,0.,0.));
#6014=DIRECTION('center_axis',(0.,0.,1.));
#6015=DIRECTION('ref_axis',(1.,0.,0.));
#6016=DIRECTION('',(0.,-1.,0.));
#6017=DIRECTION('center_axis',(-1.,0.,0.));
#6018=DIRECTION('ref_axis',(0.,0.,1.));
#6019=DIRECTION('',(0.,0.,1.));
#6020=DIRECTION('',(0.,1.,0.));
#6021=DIRECTION('',(0.,0.,-1.));
#6022=DIRECTION('',(0.,1.,0.));
#6023=DIRECTION('center_axis',(0.,0.,-1.));
#6024=DIRECTION('ref_axis',(-1.,0.,0.));
#6025=DIRECTION('',(-1.,0.,0.));
#6026=DIRECTION('',(0.,1.,0.));
#6027=DIRECTION('',(1.,0.,0.));
#6028=DIRECTION('center_axis',(1.,0.,0.));
#6029=DIRECTION('ref_axis',(0.,0.,-1.));
#6030=DIRECTION('',(0.,0.,-1.));
#6031=DIRECTION('',(0.,-1.,0.));
#6032=DIRECTION('',(0.,0.,1.));
#6033=DIRECTION('center_axis',(0.,1.,0.));
#6034=DIRECTION('ref_axis',(1.,0.,0.));
#6035=DIRECTION('center_axis',(0.,1.,0.));
#6036=DIRECTION('ref_axis',(1.,0.,0.));
#6037=DIRECTION('center_axis',(0.,-1.,0.));
#6038=DIRECTION('ref_axis',(1.,0.,0.));
#6039=DIRECTION('center_axis',(0.,1.,0.));
#6040=DIRECTION('ref_axis',(-1.83697019872103E-16,0.,1.));
#6041=DIRECTION('center_axis',(0.,-1.,0.));
#6042=DIRECTION('ref_axis',(1.,0.,0.));
#6043=DIRECTION('center_axis',(0.,1.,0.));
#6044=DIRECTION('ref_axis',(1.,0.,0.));
#6045=DIRECTION('center_axis',(0.,1.,0.));
#6046=DIRECTION('ref_axis',(1.,0.,0.));
#6047=DIRECTION('',(0.,1.,0.));
#6048=DIRECTION('center_axis',(0.,-1.,0.));
#6049=DIRECTION('ref_axis',(1.,0.,0.));
#6050=DIRECTION('center_axis',(0.,1.,0.));
#6051=DIRECTION('ref_axis',(1.,0.,0.));
#6052=DIRECTION('center_axis',(0.,1.,0.));
#6053=DIRECTION('ref_axis',(1.,0.,0.));
#6054=DIRECTION('',(0.,1.,0.));
#6055=DIRECTION('center_axis',(0.,-1.,0.));
#6056=DIRECTION('ref_axis',(1.,0.,0.));
#6057=DIRECTION('center_axis',(0.,1.,0.));
#6058=DIRECTION('ref_axis',(1.,0.,0.));
#6059=DIRECTION('center_axis',(0.,1.,0.));
#6060=DIRECTION('ref_axis',(1.,0.,0.));
#6061=DIRECTION('',(0.,1.,0.));
#6062=DIRECTION('center_axis',(0.,-1.,0.));
#6063=DIRECTION('ref_axis',(1.,0.,0.));
#6064=DIRECTION('center_axis',(0.,1.,0.));
#6065=DIRECTION('ref_axis',(1.,0.,0.));
#6066=DIRECTION('center_axis',(0.,1.,0.));
#6067=DIRECTION('ref_axis',(1.,0.,0.));
#6068=DIRECTION('',(0.,1.,0.));
#6069=DIRECTION('center_axis',(0.,-1.,0.));
#6070=DIRECTION('ref_axis',(1.,0.,0.));
#6071=DIRECTION('center_axis',(0.,1.,0.));
#6072=DIRECTION('ref_axis',(1.,0.,0.));
#6073=DIRECTION('center_axis',(0.,1.,0.));
#6074=DIRECTION('ref_axis',(1.,0.,0.));
#6075=DIRECTION('center_axis',(0.,1.,0.));
#6076=DIRECTION('ref_axis',(1.,0.,0.));
#6077=DIRECTION('center_axis',(0.,1.,0.));
#6078=DIRECTION('ref_axis',(1.,0.,0.));
#6079=DIRECTION('',(0.,-1.,0.));
#6080=DIRECTION('center_axis',(0.,1.,0.));
#6081=DIRECTION('ref_axis',(1.,0.,0.));
#6082=DIRECTION('center_axis',(0.,1.,0.));
#6083=DIRECTION('ref_axis',(1.,0.,0.));
#6084=DIRECTION('',(0.,-1.,0.));
#6085=DIRECTION('center_axis',(0.,1.,0.));
#6086=DIRECTION('ref_axis',(1.,0.,0.));
#6087=DIRECTION('axis',(0.,0.,1.));
#6088=DIRECTION('refdir',(1.,0.,0.));
#6089=DIRECTION('center_axis',(1.,0.,0.));
#6090=DIRECTION('ref_axis',(0.,0.,-1.));
#6091=DIRECTION('',(0.,-0.707106781186547,-0.707106781186548));
#6092=DIRECTION('',(0.,-1.,0.));
#6093=DIRECTION('',(0.,-0.707106781186547,0.707106781186548));
#6094=DIRECTION('',(0.,0.,1.));
#6095=DIRECTION('',(0.,0.707106781186547,0.707106781186548));
#6096=DIRECTION('',(0.,1.,0.));
#6097=DIRECTION('',(0.,0.707106781186547,-0.707106781186548));
#6098=DIRECTION('',(0.,0.,-1.));
#6099=DIRECTION('center_axis',(0.,0.707106781186548,-0.707106781186547));
#6100=DIRECTION('ref_axis',(-1.,0.,0.));
#6101=DIRECTION('',(1.,0.,0.));
#6102=DIRECTION('',(0.,-0.707106781186547,-0.707106781186548));
#6103=DIRECTION('',(-1.,0.,0.));
#6104=DIRECTION('center_axis',(0.,1.,0.));
#6105=DIRECTION('ref_axis',(-1.,0.,0.));
#6106=DIRECTION('',(-1.,0.,0.));
#6107=DIRECTION('',(0.,0.,-1.));
#6108=DIRECTION('center_axis',(0.,0.707106781186548,0.707106781186547));
#6109=DIRECTION('ref_axis',(1.,0.,0.));
#6110=DIRECTION('',(1.,0.,0.));
#6111=DIRECTION('',(0.,0.707106781186547,-0.707106781186548));
#6112=DIRECTION('center_axis',(0.,0.,1.));
#6113=DIRECTION('ref_axis',(1.,0.,0.));
#6114=DIRECTION('',(-1.,0.,0.));
#6115=DIRECTION('',(0.,1.,0.));
#6116=DIRECTION('center_axis',(1.,0.,0.));
#6117=DIRECTION('ref_axis',(0.,0.,-1.));
#6118=DIRECTION('',(0.,-0.707106781186547,0.707106781186548));
#6119=DIRECTION('',(0.,-1.,0.));
#6120=DIRECTION('',(0.,0.707106781186547,0.707106781186548));
#6121=DIRECTION('',(0.,0.,1.));
#6122=DIRECTION('center_axis',(0.,0.,1.));
#6123=DIRECTION('ref_axis',(1.,0.,0.));
#6124=DIRECTION('',(1.,0.,0.));
#6125=DIRECTION('center_axis',(0.,-0.707106781186548,0.707106781186547));
#6126=DIRECTION('ref_axis',(1.,0.,0.));
#6127=DIRECTION('',(1.,0.,0.));
#6128=DIRECTION('center_axis',(0.,-0.707106781186548,-0.707106781186547));
#6129=DIRECTION('ref_axis',(-1.,0.,0.));
#6130=DIRECTION('',(-1.,0.,0.));
#6131=DIRECTION('center_axis',(0.,-1.,0.));
#6132=DIRECTION('ref_axis',(1.,0.,0.));
#6133=DIRECTION('axis',(0.,0.,1.));
#6134=DIRECTION('refdir',(1.,0.,0.));
#6135=DIRECTION('center_axis',(0.866025403784439,0.,-0.5));
#6136=DIRECTION('ref_axis',(0.5,0.,0.866025403784439));
#6137=DIRECTION('',(0.5,0.,0.866025403784439));
#6138=DIRECTION('',(0.,-1.,0.));
#6139=DIRECTION('',(0.5,0.,0.866025403784439));
#6140=DIRECTION('',(0.,-1.,0.));
#6141=DIRECTION('center_axis',(1.92296268638356E-16,0.,-1.));
#6142=DIRECTION('ref_axis',(1.,0.,1.92296268638356E-16));
#6143=DIRECTION('',(1.,0.,1.92296268638356E-16));
#6144=DIRECTION('',(0.,-1.,0.));
#6145=DIRECTION('',(1.,0.,1.92296268638356E-16));
#6146=DIRECTION('center_axis',(-0.866025403784439,0.,-0.5));
#6147=DIRECTION('ref_axis',(0.5,0.,-0.866025403784439));
#6148=DIRECTION('',(0.5,0.,-0.866025403784439));
#6149=DIRECTION('',(0.,-1.,0.));
#6150=DIRECTION('',(0.5,0.,-0.866025403784438));
#6151=DIRECTION('center_axis',(-0.866025403784439,0.,0.5));
#6152=DIRECTION('ref_axis',(-0.5,0.,-0.866025403784439));
#6153=DIRECTION('',(-0.5,0.,-0.866025403784439));
#6154=DIRECTION('',(0.,-1.,0.));
#6155=DIRECTION('',(-0.5,0.,-0.866025403784439));
#6156=DIRECTION('center_axis',(-1.92296268638356E-16,0.,1.));
#6157=DIRECTION('ref_axis',(-1.,0.,-1.92296268638356E-16));
#6158=DIRECTION('',(-1.,0.,-1.92296268638356E-16));
#6159=DIRECTION('',(0.,-1.,0.));
#6160=DIRECTION('',(-1.,0.,-1.92296268638356E-16));
#6161=DIRECTION('center_axis',(0.866025403784439,0.,0.5));
#6162=DIRECTION('ref_axis',(-0.5,0.,0.866025403784439));
#6163=DIRECTION('',(-0.5,0.,0.866025403784439));
#6164=DIRECTION('',(-0.5,0.,0.866025403784439));
#6165=DIRECTION('center_axis',(0.,-1.,0.));
#6166=DIRECTION('ref_axis',(0.,0.,-1.));
#6167=DIRECTION('center_axis',(0.,1.,0.));
#6168=DIRECTION('ref_axis',(0.,0.,1.));
#6169=DIRECTION('center_axis',(0.,-1.,0.));
#6170=DIRECTION('ref_axis',(1.,0.,0.));
#6171=DIRECTION('center_axis',(0.,-1.,0.));
#6172=DIRECTION('ref_axis',(1.,0.,0.));
#6173=DIRECTION('center_axis',(0.,-1.,0.));
#6174=DIRECTION('ref_axis',(1.,0.,0.));
#6175=DIRECTION('',(0.707106781186547,0.707106781186548,8.65956056235493E-17));
#6176=DIRECTION('center_axis',(0.,-1.,0.));
#6177=DIRECTION('ref_axis',(1.,0.,0.));
#6178=DIRECTION('center_axis',(0.,1.,0.));
#6179=DIRECTION('ref_axis',(1.,0.,0.));
#6180=DIRECTION('',(0.,1.,0.));
#6181=DIRECTION('center_axis',(0.,1.,0.));
#6182=DIRECTION('ref_axis',(1.,0.,0.));
#6183=DIRECTION('center_axis',(0.,-1.,0.));
#6184=DIRECTION('ref_axis',(1.,0.,0.));
#6185=DIRECTION('',(-0.707106781186547,0.707106781186548,-8.65956056235493E-17));
#6186=DIRECTION('center_axis',(0.,-1.,0.));
#6187=DIRECTION('ref_axis',(0.,0.,-1.));
#6188=DIRECTION('',(0.,0.,1.));
#6189=DIRECTION('',(1.,0.,0.));
#6190=DIRECTION('',(0.,0.,1.));
#6191=DIRECTION('',(1.,0.,0.));
#6192=DIRECTION('',(0.,0.,1.));
#6193=DIRECTION('',(1.,0.,0.));
#6194=DIRECTION('',(0.,0.,1.));
#6195=DIRECTION('',(1.,0.,0.));
#6196=DIRECTION('',(0.,-1.,2.22044604925031E-16));
#6197=DIRECTION('',(1.,0.,0.));
#6198=DIRECTION('',(8.65956056235493E-17,-8.65956056235493E-17,-1.));
#6199=DIRECTION('',(2.22044604925031E-16,1.,-8.65956056235494E-17));
#6200=DIRECTION('',(0.,-1.,2.22044604925031E-16));
#6201=DIRECTION('',(1.,0.,0.));
#6202=DIRECTION('',(0.,0.,1.));
#6203=DIRECTION('',(1.,0.,0.));
#6204=DIRECTION('',(0.,0.,1.));
#6205=DIRECTION('',(1.,0.,0.));
#6206=CARTESIAN_POINT('',(0.,0.,0.));
#6207=CARTESIAN_POINT('',(0.,0.,0.));
#6208=CARTESIAN_POINT('',(0.,0.,0.));
#6209=CARTESIAN_POINT('Origin',(3.8,1.,-0.1));
#6210=CARTESIAN_POINT('',(3.55,1.,0.));
#6211=CARTESIAN_POINT('Origin',(3.8,1.,0.));
#6212=CARTESIAN_POINT('',(3.55,1.,1.));
#6213=CARTESIAN_POINT('',(3.55,1.,-0.1));
#6214=CARTESIAN_POINT('Origin',(3.8,1.,1.));
#6215=CARTESIAN_POINT('Origin',(-3.8,5.,-0.1));
#6216=CARTESIAN_POINT('',(-4.05,5.,0.));
#6217=CARTESIAN_POINT('Origin',(-3.8,5.,0.));
#6218=CARTESIAN_POINT('',(-4.05,5.,1.));
#6219=CARTESIAN_POINT('',(-4.05,5.,-0.1));
#6220=CARTESIAN_POINT('Origin',(-3.8,5.,1.));
#6221=CARTESIAN_POINT('Origin',(-3.8,1.,-0.1));
#6222=CARTESIAN_POINT('',(-4.05,1.,0.));
#6223=CARTESIAN_POINT('Origin',(-3.8,1.,0.));
#6224=CARTESIAN_POINT('',(-4.05,1.,1.));
#6225=CARTESIAN_POINT('',(-4.05,1.,-0.1));
#6226=CARTESIAN_POINT('Origin',(-3.8,1.,1.));
#6227=CARTESIAN_POINT('Origin',(3.8,5.,-0.1));
#6228=CARTESIAN_POINT('',(3.55,5.,0.));
#6229=CARTESIAN_POINT('Origin',(3.8,5.,0.));
#6230=CARTESIAN_POINT('',(3.55,5.,1.));
#6231=CARTESIAN_POINT('',(3.55,5.,-0.1));
#6232=CARTESIAN_POINT('Origin',(3.8,5.,1.));
#6233=CARTESIAN_POINT('Origin',(5.5,7.,0.));
#6234=CARTESIAN_POINT('',(5.5,7.,0.));
#6235=CARTESIAN_POINT('',(-5.5,7.,0.));
#6236=CARTESIAN_POINT('',(5.5,7.,0.));
#6237=CARTESIAN_POINT('',(-5.5,7.,1.));
#6238=CARTESIAN_POINT('',(-5.5,7.,0.));
#6239=CARTESIAN_POINT('',(5.5,7.,1.));
#6240=CARTESIAN_POINT('',(5.5,7.,1.));
#6241=CARTESIAN_POINT('',(5.5,7.,0.));
#6242=CARTESIAN_POINT('Origin',(5.5,-1.,0.));
#6243=CARTESIAN_POINT('',(5.5,-1.,0.));
#6244=CARTESIAN_POINT('',(5.5,-1.,0.));
#6245=CARTESIAN_POINT('',(5.5,-1.,1.));
#6246=CARTESIAN_POINT('',(5.5,-1.,1.));
#6247=CARTESIAN_POINT('',(5.5,-1.,0.));
#6248=CARTESIAN_POINT('Origin',(-5.5,-1.,0.));
#6249=CARTESIAN_POINT('',(-5.5,-1.,0.));
#6250=CARTESIAN_POINT('',(-5.5,-1.,0.));
#6251=CARTESIAN_POINT('',(-5.5,-1.,1.));
#6252=CARTESIAN_POINT('',(-5.5,-1.,1.));
#6253=CARTESIAN_POINT('',(-5.5,-1.,0.));
#6254=CARTESIAN_POINT('Origin',(-5.5,7.,0.));
#6255=CARTESIAN_POINT('',(-5.5,7.,0.));
#6256=CARTESIAN_POINT('',(-5.5,7.,1.));
#6257=CARTESIAN_POINT('Origin',(0.,3.,1.));
#6258=CARTESIAN_POINT('Origin',(0.,3.,0.));
#6259=CARTESIAN_POINT('',(0.,0.,0.));
#6260=CARTESIAN_POINT('Origin',(-2.8,4.4,4.5));
#6261=CARTESIAN_POINT('',(-2.965,4.4,4.5));
#6262=CARTESIAN_POINT('Origin',(-2.8,4.4,4.5));
#6263=CARTESIAN_POINT('',(-2.965,6.,4.5));
#6264=CARTESIAN_POINT('',(-2.965,4.4,4.5));
#6265=CARTESIAN_POINT('Origin',(-2.8,6.,4.5));
#6266=CARTESIAN_POINT('Origin',(-2.8,4.4,4.5));
#6267=CARTESIAN_POINT('Origin',(1.71450551880629E-16,4.4,7.3));
#6268=CARTESIAN_POINT('',(-0.165,4.4,7.3));
#6269=CARTESIAN_POINT('Origin',(1.71450551880629E-16,4.4,7.3));
#6270=CARTESIAN_POINT('',(-0.165,6.,7.3));
#6271=CARTESIAN_POINT('',(-0.165,4.4,7.3));
#6272=CARTESIAN_POINT('Origin',(1.71450551880629E-16,6.,7.3));
#6273=CARTESIAN_POINT('Origin',(1.66533453693773E-16,4.4,7.3));
#6274=CARTESIAN_POINT('Origin',(2.8,4.4,4.5));
#6275=CARTESIAN_POINT('',(2.635,4.4,4.5));
#6276=CARTESIAN_POINT('Origin',(2.8,4.4,4.5));
#6277=CARTESIAN_POINT('',(2.635,6.,4.5));
#6278=CARTESIAN_POINT('',(2.635,4.4,4.5));
#6279=CARTESIAN_POINT('Origin',(2.8,6.,4.5));
#6280=CARTESIAN_POINT('Origin',(2.8,4.4,4.5));
#6281=CARTESIAN_POINT('Origin',(-5.14351655641888E-16,4.4,1.7));
#6282=CARTESIAN_POINT('',(-0.165000000000001,4.4,1.7));
#6283=CARTESIAN_POINT('Origin',(-5.14351655641888E-16,4.4,1.7));
#6284=CARTESIAN_POINT('',(-0.165000000000001,6.,1.7));
#6285=CARTESIAN_POINT('',(-0.165000000000001,4.4,1.7));
#6286=CARTESIAN_POINT('Origin',(-5.14351655641888E-16,6.,1.7));
#6287=CARTESIAN_POINT('Origin',(-5.27355936696949E-16,4.4,1.7));
#6288=CARTESIAN_POINT('Origin',(-2.8,-0.1,4.5));
#6289=CARTESIAN_POINT('',(-2.965,0.,4.5));
#6290=CARTESIAN_POINT('Origin',(-2.8,0.,4.5));
#6291=CARTESIAN_POINT('',(-2.965,1.6,4.5));
#6292=CARTESIAN_POINT('',(-2.965,-0.1,4.5));
#6293=CARTESIAN_POINT('Origin',(-2.8,1.6,4.5));
#6294=CARTESIAN_POINT('Origin',(-2.8,1.6,4.5));
#6295=CARTESIAN_POINT('Origin',(1.71450551880629E-16,-0.1,7.3));
#6296=CARTESIAN_POINT('',(-0.165,0.,7.3));
#6297=CARTESIAN_POINT('Origin',(1.71450551880629E-16,0.,7.3));
#6298=CARTESIAN_POINT('',(-0.165,1.6,7.3));
#6299=CARTESIAN_POINT('',(-0.165,-0.1,7.3));
#6300=CARTESIAN_POINT('Origin',(1.71450551880629E-16,1.6,7.3));
#6301=CARTESIAN_POINT('Origin',(1.66533453693773E-16,1.6,7.3));
#6302=CARTESIAN_POINT('Origin',(2.8,-0.1,4.5));
#6303=CARTESIAN_POINT('',(2.635,0.,4.5));
#6304=CARTESIAN_POINT('Origin',(2.8,0.,4.5));
#6305=CARTESIAN_POINT('',(2.635,1.6,4.5));
#6306=CARTESIAN_POINT('',(2.635,-0.1,4.5));
#6307=CARTESIAN_POINT('Origin',(2.8,1.6,4.5));
#6308=CARTESIAN_POINT('Origin',(2.8,1.6,4.5));
#6309=CARTESIAN_POINT('Origin',(-5.14351655641888E-16,-0.1,1.7));
#6310=CARTESIAN_POINT('',(-0.165000000000001,0.,1.7));
#6311=CARTESIAN_POINT('Origin',(-5.14351655641888E-16,0.,1.7));
#6312=CARTESIAN_POINT('',(-0.165000000000001,1.6,1.7));
#6313=CARTESIAN_POINT('',(-0.165000000000001,-0.1,1.7));
#6314=CARTESIAN_POINT('Origin',(-5.14351655641888E-16,1.6,1.7));
#6315=CARTESIAN_POINT('Origin',(-5.27355936696949E-16,1.6,1.7));
#6316=CARTESIAN_POINT('Origin',(3.8,1.,0.9));
#6317=CARTESIAN_POINT('',(3.47,1.,1.));
#6318=CARTESIAN_POINT('Origin',(3.8,1.,1.));
#6319=CARTESIAN_POINT('',(3.47,1.,2.5));
#6320=CARTESIAN_POINT('',(3.47,1.,0.9));
#6321=CARTESIAN_POINT('Origin',(3.8,1.,2.5));
#6322=CARTESIAN_POINT('Origin',(-3.8,5.,0.9));
#6323=CARTESIAN_POINT('',(-4.13,5.,1.));
#6324=CARTESIAN_POINT('Origin',(-3.8,5.,1.));
#6325=CARTESIAN_POINT('',(-4.13,5.,2.5));
#6326=CARTESIAN_POINT('',(-4.13,5.,0.9));
#6327=CARTESIAN_POINT('Origin',(-3.8,5.,2.5));
#6328=CARTESIAN_POINT('Origin',(-3.8,1.,0.9));
#6329=CARTESIAN_POINT('',(-4.13,1.,1.));
#6330=CARTESIAN_POINT('Origin',(-3.8,1.,1.));
#6331=CARTESIAN_POINT('',(-4.13,1.,2.5));
#6332=CARTESIAN_POINT('',(-4.13,1.,0.9));
#6333=CARTESIAN_POINT('Origin',(-3.8,1.,2.5));
#6334=CARTESIAN_POINT('Origin',(3.8,5.,0.9));
#6335=CARTESIAN_POINT('',(3.47,5.,1.));
#6336=CARTESIAN_POINT('Origin',(3.8,5.,1.));
#6337=CARTESIAN_POINT('',(3.47,5.,2.5));
#6338=CARTESIAN_POINT('',(3.47,5.,0.9));
#6339=CARTESIAN_POINT('Origin',(3.8,5.,2.5));
#6340=CARTESIAN_POINT('Origin',(0.,5.5,1.75));
#6341=CARTESIAN_POINT('',(2.87228132326901,5.5,2.5));
#6342=CARTESIAN_POINT('',(0.,5.5,1.));
#6343=CARTESIAN_POINT('Origin',(0.,5.5,4.5));
#6344=CARTESIAN_POINT('',(4.5,5.5,2.5));
#6345=CARTESIAN_POINT('',(4.5,5.5,2.5));
#6346=CARTESIAN_POINT('',(4.5,5.5,1.));
#6347=CARTESIAN_POINT('',(4.5,5.5,1.));
#6348=CARTESIAN_POINT('',(-4.5,5.5,1.));
#6349=CARTESIAN_POINT('Origin',(0.,5.5,1.75));
#6350=CARTESIAN_POINT('',(-2.87228132326901,5.5,2.5));
#6351=CARTESIAN_POINT('Origin',(0.,5.5,4.5));
#6352=CARTESIAN_POINT('',(-4.5,5.5,1.));
#6353=CARTESIAN_POINT('',(-4.5,5.5,1.));
#6354=CARTESIAN_POINT('',(-4.5,5.5,2.5));
#6355=CARTESIAN_POINT('',(-4.5,5.5,2.5));
#6356=CARTESIAN_POINT('',(4.5,5.5,2.5));
#6357=CARTESIAN_POINT('Origin',(0.,4.5,1.75));
#6358=CARTESIAN_POINT('',(0.,4.5,1.));
#6359=CARTESIAN_POINT('',(2.87228132326901,4.5,2.5));
#6360=CARTESIAN_POINT('Origin',(0.,4.5,4.5));
#6361=CARTESIAN_POINT('',(4.5,4.5,1.));
#6362=CARTESIAN_POINT('',(-4.5,4.5,1.));
#6363=CARTESIAN_POINT('',(4.5,4.5,2.5));
#6364=CARTESIAN_POINT('',(4.5,4.5,1.));
#6365=CARTESIAN_POINT('',(4.5,4.5,2.5));
#6366=CARTESIAN_POINT('Origin',(0.,4.5,1.75));
#6367=CARTESIAN_POINT('',(-2.87228132326901,4.5,2.5));
#6368=CARTESIAN_POINT('Origin',(0.,4.5,4.5));
#6369=CARTESIAN_POINT('',(-4.5,4.5,2.5));
#6370=CARTESIAN_POINT('',(4.5,4.5,2.5));
#6371=CARTESIAN_POINT('',(-4.5,4.5,1.));
#6372=CARTESIAN_POINT('',(-4.5,4.5,2.5));
#6373=CARTESIAN_POINT('',(-4.5,4.5,1.));
#6374=CARTESIAN_POINT('Origin',(-4.5,4.5,2.5));
#6375=CARTESIAN_POINT('',(2.87228132326901,0.,2.5));
#6376=CARTESIAN_POINT('',(4.5,4.5,2.5));
#6377=CARTESIAN_POINT('Origin',(-4.5,4.5,2.5));
#6378=CARTESIAN_POINT('',(-2.87228132326901,0.,2.5));
#6379=CARTESIAN_POINT('',(-4.5,4.5,2.5));
#6380=CARTESIAN_POINT('Origin',(-4.5,4.5,1.));
#6381=CARTESIAN_POINT('',(-4.5,4.5,1.));
#6382=CARTESIAN_POINT('Origin',(4.5,4.5,1.));
#6383=CARTESIAN_POINT('',(4.5,4.5,1.));
#6384=CARTESIAN_POINT('Origin',(4.5,4.5,2.5));
#6385=CARTESIAN_POINT('Origin',(0.,1.5,1.75));
#6386=CARTESIAN_POINT('',(2.87228132326901,1.5,2.5));
#6387=CARTESIAN_POINT('',(0.,1.5,1.));
#6388=CARTESIAN_POINT('Origin',(0.,1.5,4.5));
#6389=CARTESIAN_POINT('',(4.5,1.5,2.5));
#6390=CARTESIAN_POINT('',(4.5,1.5,2.5));
#6391=CARTESIAN_POINT('',(4.5,1.5,1.));
#6392=CARTESIAN_POINT('',(4.5,1.5,1.));
#6393=CARTESIAN_POINT('',(-4.5,1.5,1.));
#6394=CARTESIAN_POINT('Origin',(0.,1.5,1.75));
#6395=CARTESIAN_POINT('',(-2.87228132326901,1.5,2.5));
#6396=CARTESIAN_POINT('Origin',(0.,1.5,4.5));
#6397=CARTESIAN_POINT('',(-4.5,1.5,1.));
#6398=CARTESIAN_POINT('',(-4.5,1.5,1.));
#6399=CARTESIAN_POINT('',(-4.5,1.5,2.5));
#6400=CARTESIAN_POINT('',(-4.5,1.5,2.5));
#6401=CARTESIAN_POINT('',(4.5,1.5,2.5));
#6402=CARTESIAN_POINT('Origin',(0.,0.5,1.75));
#6403=CARTESIAN_POINT('',(0.,0.5,1.));
#6404=CARTESIAN_POINT('',(2.87228132326901,0.5,2.5));
#6405=CARTESIAN_POINT('Origin',(0.,0.5,4.5));
#6406=CARTESIAN_POINT('',(4.5,0.5,1.));
#6407=CARTESIAN_POINT('',(-4.5,0.5,1.));
#6408=CARTESIAN_POINT('',(4.5,0.5,2.5));
#6409=CARTESIAN_POINT('',(4.5,0.5,1.));
#6410=CARTESIAN_POINT('',(4.5,0.5,2.5));
#6411=CARTESIAN_POINT('Origin',(0.,0.5,1.75));
#6412=CARTESIAN_POINT('',(-2.87228132326901,0.5,2.5));
#6413=CARTESIAN_POINT('Origin',(0.,0.5,4.5));
#6414=CARTESIAN_POINT('',(-4.5,0.5,2.5));
#6415=CARTESIAN_POINT('',(4.5,0.5,2.5));
#6416=CARTESIAN_POINT('',(-4.5,0.5,1.));
#6417=CARTESIAN_POINT('',(-4.5,0.5,2.5));
#6418=CARTESIAN_POINT('',(-4.5,0.5,1.));
#6419=CARTESIAN_POINT('Origin',(-4.5,0.5,2.5));
#6420=CARTESIAN_POINT('',(2.87228132326901,0.,2.5));
#6421=CARTESIAN_POINT('',(4.5,0.5,2.5));
#6422=CARTESIAN_POINT('Origin',(-4.5,0.5,2.5));
#6423=CARTESIAN_POINT('',(-2.87228132326901,0.,2.5));
#6424=CARTESIAN_POINT('',(-4.5,0.5,2.5));
#6425=CARTESIAN_POINT('Origin',(-4.5,0.5,1.));
#6426=CARTESIAN_POINT('',(-4.5,0.5,1.));
#6427=CARTESIAN_POINT('Origin',(4.5,0.5,1.));
#6428=CARTESIAN_POINT('',(4.5,0.5,1.));
#6429=CARTESIAN_POINT('Origin',(4.5,0.5,2.5));
#6430=CARTESIAN_POINT('Origin',(0.,0.,4.5));
#6431=CARTESIAN_POINT('',(-2.35,6.,4.5));
#6432=CARTESIAN_POINT('Origin',(0.,6.,4.5));
#6433=CARTESIAN_POINT('',(-2.35,0.,4.5));
#6434=CARTESIAN_POINT('',(-2.35,0.,4.5));
#6435=CARTESIAN_POINT('Origin',(0.,0.,4.5));
#6436=CARTESIAN_POINT('Origin',(0.,0.,4.5));
#6437=CARTESIAN_POINT('',(-3.5,6.,4.5));
#6438=CARTESIAN_POINT('Origin',(0.,6.,4.5));
#6439=CARTESIAN_POINT('',(-3.5,0.,4.5));
#6440=CARTESIAN_POINT('',(-3.5,0.,4.5));
#6441=CARTESIAN_POINT('Origin',(0.,0.,4.5));
#6442=CARTESIAN_POINT('Origin',(0.,6.,4.5));
#6443=CARTESIAN_POINT('Origin',(0.,0.,4.5));
#6444=CARTESIAN_POINT('',(0.,0.,0.));
#6445=CARTESIAN_POINT('Origin',(0.,1.7,4.5));
#6446=CARTESIAN_POINT('',(-1.75,4.3,4.5));
#6447=CARTESIAN_POINT('Origin',(0.,4.3,4.5));
#6448=CARTESIAN_POINT('',(-1.75,1.7,4.5));
#6449=CARTESIAN_POINT('',(-1.75,1.7,4.5));
#6450=CARTESIAN_POINT('Origin',(0.,1.7,4.5));
#6451=CARTESIAN_POINT('Origin',(0.,1.7,4.5));
#6452=CARTESIAN_POINT('',(-2.34,4.3,4.5));
#6453=CARTESIAN_POINT('Origin',(0.,4.3,4.5));
#6454=CARTESIAN_POINT('',(-2.34,1.7,4.5));
#6455=CARTESIAN_POINT('',(-2.34,1.7,4.5));
#6456=CARTESIAN_POINT('Origin',(0.,1.7,4.5));
#6457=CARTESIAN_POINT('Origin',(0.,4.3,4.5));
#6458=CARTESIAN_POINT('Origin',(0.,1.7,4.5));
#6459=CARTESIAN_POINT('',(0.,0.,0.));
#6460=CARTESIAN_POINT('Origin',(-2.8,-0.5,4.5));
#6461=CARTESIAN_POINT('',(-3.025,-0.4,4.5));
#6462=CARTESIAN_POINT('Origin',(-2.8,-0.4,4.5));
#6463=CARTESIAN_POINT('',(-3.025,0.,4.5));
#6464=CARTESIAN_POINT('',(-3.025,-0.5,4.5));
#6465=CARTESIAN_POINT('Origin',(-2.8,0.,4.5));
#6466=CARTESIAN_POINT('Origin',(1.71450551880629E-16,-0.5,7.3));
#6467=CARTESIAN_POINT('',(-0.225,-0.4,7.3));
#6468=CARTESIAN_POINT('Origin',(1.71450551880629E-16,-0.4,7.3));
#6469=CARTESIAN_POINT('',(-0.225,0.,7.3));
#6470=CARTESIAN_POINT('',(-0.225,-0.5,7.3));
#6471=CARTESIAN_POINT('Origin',(1.71450551880629E-16,0.,7.3));
#6472=CARTESIAN_POINT('Origin',(2.8,-0.5,4.5));
#6473=CARTESIAN_POINT('',(2.575,-0.4,4.5));
#6474=CARTESIAN_POINT('Origin',(2.8,-0.4,4.5));
#6475=CARTESIAN_POINT('',(2.575,0.,4.5));
#6476=CARTESIAN_POINT('',(2.575,-0.5,4.5));
#6477=CARTESIAN_POINT('Origin',(2.8,0.,4.5));
#6478=CARTESIAN_POINT('Origin',(-5.14351655641888E-16,-0.5,1.7));
#6479=CARTESIAN_POINT('',(-0.225000000000001,-0.4,1.7));
#6480=CARTESIAN_POINT('Origin',(-5.14351655641888E-16,-0.4,1.7));
#6481=CARTESIAN_POINT('',(-0.225000000000001,0.,1.7));
#6482=CARTESIAN_POINT('',(-0.225000000000001,-0.5,1.7));
#6483=CARTESIAN_POINT('Origin',(-5.14351655641888E-16,0.,1.7));
#6484=CARTESIAN_POINT('Origin',(0.,0.,4.5));
#6485=CARTESIAN_POINT('',(-2.34,0.3,4.5));
#6486=CARTESIAN_POINT('Origin',(0.,0.3,4.5));
#6487=CARTESIAN_POINT('',(-2.34,0.,4.5));
#6488=CARTESIAN_POINT('',(-2.34,0.,4.5));
#6489=CARTESIAN_POINT('Origin',(0.,0.,4.5));
#6490=CARTESIAN_POINT('Origin',(0.,0.3,4.5));
#6491=CARTESIAN_POINT('',(-1.6,0.3,4.5));
#6492=CARTESIAN_POINT('Origin',(0.,0.3,4.5));
#6493=CARTESIAN_POINT('Origin',(0.,-0.41,4.5));
#6494=CARTESIAN_POINT('',(-1.8,-0.4,4.5));
#6495=CARTESIAN_POINT('Origin',(0.,-0.4,4.5));
#6496=CARTESIAN_POINT('',(-1.8,-0.2,4.5));
#6497=CARTESIAN_POINT('',(-1.8,-0.41,4.5));
#6498=CARTESIAN_POINT('Origin',(0.,-0.2,4.5));
#6499=CARTESIAN_POINT('Origin',(0.,-0.2,4.5));
#6500=CARTESIAN_POINT('',(-1.6,-0.2,4.5));
#6501=CARTESIAN_POINT('Origin',(0.,-0.2,4.5));
#6502=CARTESIAN_POINT('Origin',(0.,-0.4,4.5));
#6503=CARTESIAN_POINT('',(-1.6,-0.4,4.5));
#6504=CARTESIAN_POINT('Origin',(0.,-0.4,4.5));
#6505=CARTESIAN_POINT('',(-3.5,0.,4.5));
#6506=CARTESIAN_POINT('Origin',(0.,0.,4.5));
#6507=CARTESIAN_POINT('',(-3.5,-0.4,4.5));
#6508=CARTESIAN_POINT('',(-3.5,-0.4,4.5));
#6509=CARTESIAN_POINT('Origin',(0.,-0.4,4.5));
#6510=CARTESIAN_POINT('Origin',(0.,0.,4.5));
#6511=CARTESIAN_POINT('Origin',(0.,-0.4,4.5));
#6512=CARTESIAN_POINT('',(0.,0.,0.));
#6513=CARTESIAN_POINT('Origin',(0.,-0.4,4.5));
#6514=CARTESIAN_POINT('',(-1.,-0.2,4.5));
#6515=CARTESIAN_POINT('Origin',(0.,-0.2,4.5));
#6516=CARTESIAN_POINT('',(-1.,-0.4,4.5));
#6517=CARTESIAN_POINT('',(-1.,-0.4,4.5));
#6518=CARTESIAN_POINT('Origin',(0.,-0.4,4.5));
#6519=CARTESIAN_POINT('Origin',(0.,-0.4,4.5));
#6520=CARTESIAN_POINT('',(-1.8,-0.2,4.5));
#6521=CARTESIAN_POINT('Origin',(0.,-0.2,4.5));
#6522=CARTESIAN_POINT('',(-1.8,-0.4,4.5));
#6523=CARTESIAN_POINT('',(-1.8,-0.4,4.5));
#6524=CARTESIAN_POINT('Origin',(0.,-0.4,4.5));
#6525=CARTESIAN_POINT('Origin',(0.,-0.2,4.5));
#6526=CARTESIAN_POINT('Origin',(0.,-0.4,4.5));
#6527=CARTESIAN_POINT('',(0.,0.,0.));
#6528=CARTESIAN_POINT('Origin',(-2.8,6.4,4.5));
#6529=CARTESIAN_POINT('',(-3.2,6.4,4.5));
#6530=CARTESIAN_POINT('Origin',(-2.8,6.4,4.5));
#6531=CARTESIAN_POINT('',(-3.2,7.3,4.5));
#6532=CARTESIAN_POINT('',(-3.2,6.4,4.5));
#6533=CARTESIAN_POINT('Origin',(-2.8,7.3,4.5));
#6534=CARTESIAN_POINT('Origin',(-2.8,6.4,4.5));
#6535=CARTESIAN_POINT('',(-3.025,6.4,4.5));
#6536=CARTESIAN_POINT('Origin',(-2.8,6.4,4.5));
#6537=CARTESIAN_POINT('Origin',(1.71450551880629E-16,6.4,7.3));
#6538=CARTESIAN_POINT('',(-0.4,6.4,7.3));
#6539=CARTESIAN_POINT('Origin',(1.71450551880629E-16,6.4,7.3));
#6540=CARTESIAN_POINT('',(-0.4,7.3,7.3));
#6541=CARTESIAN_POINT('',(-0.4,6.4,7.3));
#6542=CARTESIAN_POINT('Origin',(1.71450551880629E-16,7.3,7.3));
#6543=CARTESIAN_POINT('Origin',(1.66533453693773E-16,6.4,7.3));
#6544=CARTESIAN_POINT('',(-0.225,6.4,7.3));
#6545=CARTESIAN_POINT('Origin',(1.71450551880629E-16,6.4,7.3));
#6546=CARTESIAN_POINT('Origin',(2.8,6.4,4.5));
#6547=CARTESIAN_POINT('',(2.4,6.4,4.5));
#6548=CARTESIAN_POINT('Origin',(2.8,6.4,4.5));
#6549=CARTESIAN_POINT('',(2.4,7.3,4.5));
#6550=CARTESIAN_POINT('',(2.4,6.4,4.5));
#6551=CARTESIAN_POINT('Origin',(2.8,7.3,4.5));
#6552=CARTESIAN_POINT('Origin',(2.8,6.4,4.5));
#6553=CARTESIAN_POINT('',(2.575,6.4,4.5));
#6554=CARTESIAN_POINT('Origin',(2.8,6.4,4.5));
#6555=CARTESIAN_POINT('Origin',(-5.14351655641888E-16,6.4,1.7));
#6556=CARTESIAN_POINT('',(-0.400000000000001,6.4,1.7));
#6557=CARTESIAN_POINT('Origin',(-5.14351655641888E-16,6.4,1.7));
#6558=CARTESIAN_POINT('',(-0.400000000000001,7.3,1.7));
#6559=CARTESIAN_POINT('',(-0.400000000000001,6.4,1.7));
#6560=CARTESIAN_POINT('Origin',(-5.14351655641888E-16,7.3,1.7));
#6561=CARTESIAN_POINT('Origin',(-4.9960036108132E-16,6.4,1.7));
#6562=CARTESIAN_POINT('',(-0.225000000000001,6.4,1.7));
#6563=CARTESIAN_POINT('Origin',(-5.14351655641888E-16,6.4,1.7));
#6564=CARTESIAN_POINT('Origin',(-2.8,5.9,4.5));
#6565=CARTESIAN_POINT('',(-3.025,6.,4.5));
#6566=CARTESIAN_POINT('Origin',(-2.8,6.,4.5));
#6567=CARTESIAN_POINT('',(-3.025,5.9,4.5));
#6568=CARTESIAN_POINT('Origin',(1.71450551880629E-16,5.9,7.3));
#6569=CARTESIAN_POINT('',(-0.225,6.,7.3));
#6570=CARTESIAN_POINT('Origin',(1.71450551880629E-16,6.,7.3));
#6571=CARTESIAN_POINT('',(-0.225,5.9,7.3));
#6572=CARTESIAN_POINT('Origin',(2.8,5.9,4.5));
#6573=CARTESIAN_POINT('',(2.575,6.,4.5));
#6574=CARTESIAN_POINT('Origin',(2.8,6.,4.5));
#6575=CARTESIAN_POINT('',(2.575,5.9,4.5));
#6576=CARTESIAN_POINT('Origin',(-5.14351655641888E-16,5.9,1.7));
#6577=CARTESIAN_POINT('',(-0.225000000000001,6.,1.7));
#6578=CARTESIAN_POINT('Origin',(-5.14351655641888E-16,6.,1.7));
#6579=CARTESIAN_POINT('',(-0.225000000000001,5.9,1.7));
#6580=CARTESIAN_POINT('Origin',(0.,6.,4.5));
#6581=CARTESIAN_POINT('',(-2.,6.,4.5));
#6582=CARTESIAN_POINT('Origin',(0.,6.,4.5));
#6583=CARTESIAN_POINT('',(-1.8,6.,4.5));
#6584=CARTESIAN_POINT('Origin',(0.,6.,4.5));
#6585=CARTESIAN_POINT('Origin',(0.,5.7,4.5));
#6586=CARTESIAN_POINT('',(-1.8,5.7,4.5));
#6587=CARTESIAN_POINT('',(-1.8,5.7,4.5));
#6588=CARTESIAN_POINT('Origin',(0.,5.7,4.5));
#6589=CARTESIAN_POINT('Origin',(0.,5.7,4.5));
#6590=CARTESIAN_POINT('',(-2.34,6.,4.5));
#6591=CARTESIAN_POINT('Origin',(0.,6.,4.5));
#6592=CARTESIAN_POINT('',(-2.34,5.7,4.5));
#6593=CARTESIAN_POINT('',(-2.34,5.7,4.5));
#6594=CARTESIAN_POINT('Origin',(0.,5.7,4.5));
#6595=CARTESIAN_POINT('Origin',(0.,5.7,4.5));
#6596=CARTESIAN_POINT('Origin',(0.,5.9,4.5));
#6597=CARTESIAN_POINT('',(-2.,6.9,4.5));
#6598=CARTESIAN_POINT('',(-2.,5.9,4.5));
#6599=CARTESIAN_POINT('Origin',(0.,6.9,4.5));
#6600=CARTESIAN_POINT('Origin',(0.,6.9,4.5));
#6601=CARTESIAN_POINT('Origin',(0.,6.,4.5));
#6602=CARTESIAN_POINT('',(-3.5,7.3,4.5));
#6603=CARTESIAN_POINT('Origin',(0.,7.3,4.5));
#6604=CARTESIAN_POINT('',(-3.5,6.,4.5));
#6605=CARTESIAN_POINT('',(-3.5,6.,4.5));
#6606=CARTESIAN_POINT('Origin',(0.,6.,4.5));
#6607=CARTESIAN_POINT('Origin',(0.,7.3,4.5));
#6608=CARTESIAN_POINT('Origin',(0.,6.,4.5));
#6609=CARTESIAN_POINT('',(0.,0.,0.));
#6610=CARTESIAN_POINT('Origin',(5.5,0.,-0.3));
#6611=CARTESIAN_POINT('',(5.5,0.,-0.3));
#6612=CARTESIAN_POINT('',(-5.5,0.,-0.3));
#6613=CARTESIAN_POINT('',(5.5,0.,-0.3));
#6614=CARTESIAN_POINT('',(-5.5,0.,0.));
#6615=CARTESIAN_POINT('',(-5.5,0.,-0.3));
#6616=CARTESIAN_POINT('',(5.5,0.,0.));
#6617=CARTESIAN_POINT('',(5.5,0.,0.));
#6618=CARTESIAN_POINT('',(5.5,0.,-0.3));
#6619=CARTESIAN_POINT('Origin',(5.5,-1.,-0.3));
#6620=CARTESIAN_POINT('',(5.5,-1.,-0.3));
#6621=CARTESIAN_POINT('',(5.5,-1.,-0.3));
#6622=CARTESIAN_POINT('',(5.5,-1.,0.));
#6623=CARTESIAN_POINT('',(5.5,-1.,0.));
#6624=CARTESIAN_POINT('',(5.5,-1.,-0.3));
#6625=CARTESIAN_POINT('Origin',(-5.5,-1.,-0.3));
#6626=CARTESIAN_POINT('',(-5.5,-1.,-0.3));
#6627=CARTESIAN_POINT('',(-5.5,-1.,-0.3));
#6628=CARTESIAN_POINT('',(-5.5,-1.,0.));
#6629=CARTESIAN_POINT('',(-5.5,-1.,0.));
#6630=CARTESIAN_POINT('',(-5.5,-1.,-0.3));
#6631=CARTESIAN_POINT('Origin',(-5.5,0.,-0.3));
#6632=CARTESIAN_POINT('',(-5.5,0.,-0.3));
#6633=CARTESIAN_POINT('',(-5.5,0.,0.));
#6634=CARTESIAN_POINT('Origin',(0.,-0.5,0.));
#6635=CARTESIAN_POINT('Origin',(0.,-0.5,-0.3));
#6636=CARTESIAN_POINT('',(0.,0.,0.));
#6637=CARTESIAN_POINT('Origin',(5.5,7.,-0.3));
#6638=CARTESIAN_POINT('',(5.5,7.,-0.3));
#6639=CARTESIAN_POINT('',(-5.5,7.,-0.3));
#6640=CARTESIAN_POINT('',(5.5,7.,-0.3));
#6641=CARTESIAN_POINT('',(-5.5,7.,0.));
#6642=CARTESIAN_POINT('',(-5.5,7.,-0.3));
#6643=CARTESIAN_POINT('',(5.5,7.,0.));
#6644=CARTESIAN_POINT('',(5.5,7.,0.));
#6645=CARTESIAN_POINT('',(5.5,7.,-0.3));
#6646=CARTESIAN_POINT('Origin',(5.5,6.,-0.3));
#6647=CARTESIAN_POINT('',(5.5,6.,-0.3));
#6648=CARTESIAN_POINT('',(5.5,6.,-0.3));
#6649=CARTESIAN_POINT('',(5.5,6.,0.));
#6650=CARTESIAN_POINT('',(5.5,6.,0.));
#6651=CARTESIAN_POINT('',(5.5,6.,-0.3));
#6652=CARTESIAN_POINT('Origin',(-5.5,6.,-0.3));
#6653=CARTESIAN_POINT('',(-5.5,6.,-0.3));
#6654=CARTESIAN_POINT('',(-5.5,6.,-0.3));
#6655=CARTESIAN_POINT('',(-5.5,6.,0.));
#6656=CARTESIAN_POINT('',(-5.5,6.,0.));
#6657=CARTESIAN_POINT('',(-5.5,6.,-0.3));
#6658=CARTESIAN_POINT('Origin',(-5.5,7.,-0.3));
#6659=CARTESIAN_POINT('',(-5.5,7.,-0.3));
#6660=CARTESIAN_POINT('',(-5.5,7.,0.));
#6661=CARTESIAN_POINT('Origin',(0.,6.5,0.));
#6662=CARTESIAN_POINT('Origin',(0.,6.5,-0.3));
#6663=CARTESIAN_POINT('',(0.,0.,0.));
#6664=CARTESIAN_POINT('',(0.,0.,0.));
#6665=CARTESIAN_POINT('Origin',(0.,0.,0.));
#6666=CARTESIAN_POINT('',(-1.63531,-0.410863395882378,-2.00267715711366E-16));
#6667=CARTESIAN_POINT('',(-2.00267715711366E-16,-0.410863395882378,1.63531));
#6668=CARTESIAN_POINT('Origin',(0.,-0.410863395882378,0.));
#6669=CARTESIAN_POINT('Origin',(0.,-0.410863395882378,0.));
#6670=CARTESIAN_POINT('',(-2.00267715711366E-16,0.410863395882378,1.63531));
#6671=CARTESIAN_POINT('Origin',(-2.05128338857182E-16,0.,1.675));
#6672=CARTESIAN_POINT('',(-1.63531,0.410863395882378,2.00267715711366E-16));
#6673=CARTESIAN_POINT('Origin',(0.,0.410863395882378,0.));
#6674=CARTESIAN_POINT('Origin',(0.,0.410863395882378,0.));
#6675=CARTESIAN_POINT('Origin',(0.,0.,0.));
#6676=CARTESIAN_POINT('',(-1.63531,0.7,-2.00267715711366E-16));
#6677=CARTESIAN_POINT('',(-1.63531,0.,-2.00267715711366E-16));
#6678=CARTESIAN_POINT('Origin',(0.,0.7,0.));
#6679=CARTESIAN_POINT('Origin',(0.,0.,0.));
#6680=CARTESIAN_POINT('',(-1.,-0.6,-1.22464679914735E-16));
#6681=CARTESIAN_POINT('Origin',(0.,-0.6,0.));
#6682=CARTESIAN_POINT('',(-1.,0.6,-1.22464679914735E-16));
#6683=CARTESIAN_POINT('',(-1.,0.,-1.22464679914735E-16));
#6684=CARTESIAN_POINT('Origin',(0.,0.6,0.));
#6685=CARTESIAN_POINT('Origin',(0.,0.65,0.));
#6686=CARTESIAN_POINT('',(-1.1,0.7,-1.34711147906209E-16));
#6687=CARTESIAN_POINT('',(-1.05,0.65,-1.28587913910472E-16));
#6688=CARTESIAN_POINT('Origin',(0.,0.7,0.));
#6689=CARTESIAN_POINT('Origin',(1.63531,0.7,0.));
#6690=CARTESIAN_POINT('Origin',(0.,0.,0.));
#6691=CARTESIAN_POINT('',(-1.63531,-0.7,-2.00267715711366E-16));
#6692=CARTESIAN_POINT('Origin',(0.,-0.7,0.));
#6693=CARTESIAN_POINT('',(-1.63531,0.,-2.00267715711366E-16));
#6694=CARTESIAN_POINT('Origin',(1.1,-0.7,0.));
#6695=CARTESIAN_POINT('',(-1.1,-0.7,-1.34711147906209E-16));
#6696=CARTESIAN_POINT('Origin',(0.,-0.7,0.));
#6697=CARTESIAN_POINT('Origin',(0.,-0.65,0.));
#6698=CARTESIAN_POINT('',(-1.05,-0.65,-1.28587913910472E-16));
#6699=CARTESIAN_POINT('',(0.,0.,0.));
#6700=CARTESIAN_POINT('Origin',(0.,0.,0.));
#6701=CARTESIAN_POINT('',(-1.71469,0.410863395882378,-2.09988962002998E-16));
#6702=CARTESIAN_POINT('',(-2.09988962002998E-16,0.410863395882378,1.71469));
#6703=CARTESIAN_POINT('Origin',(0.,0.410863395882378,0.));
#6704=CARTESIAN_POINT('Origin',(0.,0.410863395882378,0.));
#6705=CARTESIAN_POINT('',(-2.09988962002998E-16,-0.410863395882378,1.71469));
#6706=CARTESIAN_POINT('Origin',(-2.05128338857182E-16,0.,1.675));
#6707=CARTESIAN_POINT('',(-1.71469,-0.410863395882378,2.09988962002998E-16));
#6708=CARTESIAN_POINT('Origin',(0.,-0.410863395882378,0.));
#6709=CARTESIAN_POINT('Origin',(0.,-0.410863395882378,0.));
#6710=CARTESIAN_POINT('Origin',(0.,0.,0.));
#6711=CARTESIAN_POINT('',(-1.71469,-0.7,-2.09988962002998E-16));
#6712=CARTESIAN_POINT('Origin',(0.,-0.7,0.));
#6713=CARTESIAN_POINT('',(-1.71469,0.,-2.09988962002998E-16));
#6714=CARTESIAN_POINT('Origin',(2.25,0.7,0.));
#6715=CARTESIAN_POINT('',(-2.25,0.7,-2.75545529808154E-16));
#6716=CARTESIAN_POINT('Origin',(0.,0.7,0.));
#6717=CARTESIAN_POINT('',(-1.71469,0.7,-2.09988962002998E-16));
#6718=CARTESIAN_POINT('Origin',(0.,0.7,0.));
#6719=CARTESIAN_POINT('Origin',(0.,0.65,0.));
#6720=CARTESIAN_POINT('',(-2.35,0.6,-2.87791997799628E-16));
#6721=CARTESIAN_POINT('Origin',(0.,0.6,0.));
#6722=CARTESIAN_POINT('',(-2.3,0.65,-2.81668763803891E-16));
#6723=CARTESIAN_POINT('Origin',(0.,0.,0.));
#6724=CARTESIAN_POINT('',(-2.35,-0.6,-2.87791997799628E-16));
#6725=CARTESIAN_POINT('Origin',(0.,-0.6,0.));
#6726=CARTESIAN_POINT('',(-2.35,0.,-2.87791997799628E-16));
#6727=CARTESIAN_POINT('Origin',(0.,-0.65,0.));
#6728=CARTESIAN_POINT('',(-2.25,-0.7,-2.75545529808154E-16));
#6729=CARTESIAN_POINT('Origin',(0.,-0.7,0.));
#6730=CARTESIAN_POINT('',(-2.3,-0.65,-2.81668763803891E-16));
#6731=CARTESIAN_POINT('Origin',(1.71469,-0.7,0.));
#6732=CARTESIAN_POINT('Origin',(0.,0.,0.));
#6733=CARTESIAN_POINT('',(-1.71469,0.,-2.09988962002998E-16));
#6734=CARTESIAN_POINT('',(0.,0.,0.));
#6735=CARTESIAN_POINT('Origin',(1.675,0.,0.));
#6736=CARTESIAN_POINT('',(1.675,-2.97627328869245E-33,0.3969));
#6737=CARTESIAN_POINT('',(1.675,-2.97627328869245E-33,-0.3969));
#6738=CARTESIAN_POINT('Origin',(1.675,0.,0.));
#6739=CARTESIAN_POINT('Origin',(1.18440385848747,0.,-1.18440385848747));
#6740=CARTESIAN_POINT('',(1.46505453994041,3.1867025333467E-33,-0.903753177034526));
#6741=CARTESIAN_POINT('',(0.903753177034527,-9.13924911073161E-33,-1.46505453994041));
#6742=CARTESIAN_POINT('Origin',(1.18440385848747,0.,-1.18440385848747));
#6743=CARTESIAN_POINT('Origin',(1.02564169428591E-16,0.,-1.675));
#6744=CARTESIAN_POINT('',(0.3969,-2.97627328869246E-33,-1.675));
#6745=CARTESIAN_POINT('',(-0.3969,-2.97627328869245E-33,-1.675));
#6746=CARTESIAN_POINT('Origin',(1.02564169428591E-16,0.,-1.675));
#6747=CARTESIAN_POINT('Origin',(-1.18440385848747,0.,-1.18440385848747));
#6748=CARTESIAN_POINT('',(-0.903753177034526,3.1867025333467E-33,-1.46505453994041));
#6749=CARTESIAN_POINT('',(-1.46505453994041,-9.13924911073161E-33,-0.903753177034527));
#6750=CARTESIAN_POINT('Origin',(-1.18440385848747,0.,-1.18440385848747));
#6751=CARTESIAN_POINT('Origin',(-1.675,0.,-2.05128338857182E-16));
#6752=CARTESIAN_POINT('',(-1.675,-2.97627328869246E-33,-0.3969));
#6753=CARTESIAN_POINT('',(-1.675,-2.97627328869245E-33,0.3969));
#6754=CARTESIAN_POINT('Origin',(-1.675,0.,-2.05128338857182E-16));
#6755=CARTESIAN_POINT('Origin',(-1.18440385848747,0.,1.18440385848747));
#6756=CARTESIAN_POINT('',(-1.46505453994041,6.26819044436628E-33,0.903753177034526));
#6757=CARTESIAN_POINT('',(-0.903753177034527,-1.22207370217512E-32,1.46505453994041));
#6758=CARTESIAN_POINT('Origin',(-1.18440385848747,0.,1.18440385848747));
#6759=CARTESIAN_POINT('Origin',(-3.07692508285772E-16,0.,1.675));
#6760=CARTESIAN_POINT('',(-0.3969,-2.97627328869246E-33,1.675));
#6761=CARTESIAN_POINT('',(0.396899999999999,-2.97627328869245E-33,1.675));
#6762=CARTESIAN_POINT('Origin',(-3.07692508285772E-16,0.,1.675));
#6763=CARTESIAN_POINT('Origin',(1.18440385848747,0.,1.18440385848747));
#6764=CARTESIAN_POINT('',(0.903753177034526,9.34967835538585E-33,1.46505453994041));
#6765=CARTESIAN_POINT('',(1.46505453994041,-1.53022249327708E-32,0.903753177034527));
#6766=CARTESIAN_POINT('Origin',(1.18440385848747,0.,1.18440385848747));
#6767=CARTESIAN_POINT('',(0.,0.,0.));
#6768=CARTESIAN_POINT('Origin',(1.18440385848747,0.,1.18440385848747));
#6769=CARTESIAN_POINT('',(0.846804978391753,-0.07938,1.40825612658882));
#6770=CARTESIAN_POINT('',(1.40825612658882,-0.07938,0.846804978391754));
#6771=CARTESIAN_POINT('Ctrl Pts',(0.846804978391752,-0.0793800000000001,
1.40825612658882));
#6772=CARTESIAN_POINT('Ctrl Pts',(0.854205272175554,-0.123401821157026,
1.40380622184538));
#6773=CARTESIAN_POINT('Ctrl Pts',(0.867957148219441,-0.166543350814306,
1.39550172959303));
#6774=CARTESIAN_POINT('Ctrl Pts',(0.902193646979982,-0.237231147975234,
1.3735491215176));
#6775=CARTESIAN_POINT('Ctrl Pts',(0.920778333482564,-0.266264900654909,
1.36127834356734));
#6776=CARTESIAN_POINT('Ctrl Pts',(0.962485392528369,-0.317195968905306,
1.33211611256184));
#6777=CARTESIAN_POINT('Ctrl Pts',(0.985600426557816,-0.33909093068465,1.31521005565926));
#6778=CARTESIAN_POINT('Ctrl Pts',(1.03253285680459,-0.373586846396559,1.27866649102984));
#6779=CARTESIAN_POINT('Ctrl Pts',(1.05871835910697,-0.388086240756494,1.25722555095714));
#6780=CARTESIAN_POINT('Ctrl Pts',(1.11153475808518,-0.407068917407805,1.2107812086231));
#6781=CARTESIAN_POINT('Ctrl Pts',(1.13814686046673,-0.411552957311693,1.18575674747573));
#6782=CARTESIAN_POINT('Ctrl Pts',(1.18575674747573,-0.411552957311693,1.13814686046673));
#6783=CARTESIAN_POINT('Ctrl Pts',(1.2107812086231,-0.407068917407805,1.11153475808518));
#6784=CARTESIAN_POINT('Ctrl Pts',(1.25722555095713,-0.388086240756494,1.05871835910697));
#6785=CARTESIAN_POINT('Ctrl Pts',(1.27866649102984,-0.373586846396559,1.03253285680459));
#6786=CARTESIAN_POINT('Ctrl Pts',(1.31521005565926,-0.33909093068465,0.985600426557816));
#6787=CARTESIAN_POINT('Ctrl Pts',(1.33211611256184,-0.317195968905306,0.962485392528369));
#6788=CARTESIAN_POINT('Ctrl Pts',(1.36127834356734,-0.266264900654909,0.920778333482565));
#6789=CARTESIAN_POINT('Ctrl Pts',(1.3735491215176,-0.237231147975234,0.902193646979983));
#6790=CARTESIAN_POINT('Ctrl Pts',(1.39550172959303,-0.166543350814306,0.867957148219442));
#6791=CARTESIAN_POINT('Ctrl Pts',(1.40380622184538,-0.123401821157026,0.854205272175555));
#6792=CARTESIAN_POINT('Ctrl Pts',(1.40825612658882,-0.0793800000000001,
0.846804978391753));
#6793=CARTESIAN_POINT('',(0.886256117232623,-0.07938,1.45861320581289));
#6794=CARTESIAN_POINT('Origin',(1.18440385848747,-0.07938,1.18440385848747));
#6795=CARTESIAN_POINT('',(1.45861320581289,-0.07938,0.886256117232624));
#6796=CARTESIAN_POINT('Ctrl Pts',(1.45861320581289,-0.0793800000000001,
0.886256117232623));
#6797=CARTESIAN_POINT('Ctrl Pts',(1.45630208793976,-0.101649918886749,0.890059788636852));
#6798=CARTESIAN_POINT('Ctrl Pts',(1.45296717977858,-0.123823518623746,0.895520212222107));
#6799=CARTESIAN_POINT('Ctrl Pts',(1.43904931717599,-0.192480977588836,0.917859913453975));
#6800=CARTESIAN_POINT('Ctrl Pts',(1.4243271592157,-0.236152929235938,0.940896403863072));
#6801=CARTESIAN_POINT('Ctrl Pts',(1.39055359345152,-0.303141259068212,0.990027513266106));
#6802=CARTESIAN_POINT('Ctrl Pts',(1.36743459453896,-0.335108247315849,1.02199477007745));
#6803=CARTESIAN_POINT('Ctrl Pts',(1.32643091652006,-0.373243761060364,1.07446535104584));
#6804=CARTESIAN_POINT('Ctrl Pts',(1.30441816675528,-0.387888272594439,1.10126842659597));
#6805=CARTESIAN_POINT('Ctrl Pts',(1.25681160160691,-0.407041111792943,1.15530234155453));
#6806=CARTESIAN_POINT('Ctrl Pts',(1.23119764287622,-0.411552957311693,1.18251418313119));
#6807=CARTESIAN_POINT('Ctrl Pts',(1.18251418313119,-0.411552957311693,1.23119764287622));
#6808=CARTESIAN_POINT('Ctrl Pts',(1.15530234155453,-0.407041111792943,1.25681160160691));
#6809=CARTESIAN_POINT('Ctrl Pts',(1.10126842659597,-0.387888272594439,1.30441816675528));
#6810=CARTESIAN_POINT('Ctrl Pts',(1.07446535104584,-0.373243761060364,1.32643091652006));
#6811=CARTESIAN_POINT('Ctrl Pts',(1.02199477007745,-0.335108247315848,1.36743459453896));
#6812=CARTESIAN_POINT('Ctrl Pts',(0.990027513266105,-0.303141259068211,
1.39055359345152));
#6813=CARTESIAN_POINT('Ctrl Pts',(0.940896403863071,-0.236152929235937,
1.42432715921571));
#6814=CARTESIAN_POINT('Ctrl Pts',(0.917859913453974,-0.192480977588835,
1.43904931717599));
#6815=CARTESIAN_POINT('Ctrl Pts',(0.895520212222106,-0.123823518623745,
1.45296717977858));
#6816=CARTESIAN_POINT('Ctrl Pts',(0.890059788636851,-0.101649918886749,
1.45630208793976));
#6817=CARTESIAN_POINT('Ctrl Pts',(0.886256117232622,-0.0793800000000001,
1.45861320581289));
#6818=CARTESIAN_POINT('Origin',(1.18440385848747,-0.07938,1.18440385848747));
#6819=CARTESIAN_POINT('Origin',(0.,-0.27783,0.));
#6820=CARTESIAN_POINT('',(0.404717578595295,-0.07938,1.65807299932179));
#6821=CARTESIAN_POINT('Origin',(0.,-0.07938,0.));
#6822=CARTESIAN_POINT('',(-0.404717578595296,-0.07938,1.65807299932179));
#6823=CARTESIAN_POINT('Ctrl Pts',(0.404717578595296,-0.0793800000000001,
1.65807299932179));
#6824=CARTESIAN_POINT('Ctrl Pts',(0.400393769631747,-0.101649918886749,
1.65912839404491));
#6825=CARTESIAN_POINT('Ctrl Pts',(0.394174530911058,-0.123823518623745,
1.66063136041479));
#6826=CARTESIAN_POINT('Ctrl Pts',(0.368536561654407,-0.192480977588835,
1.66658649961961));
#6827=CARTESIAN_POINT('Ctrl Pts',(0.341837165343982,-0.236152929235937,
1.67246562047521));
#6828=CARTESIAN_POINT('Ctrl Pts',(0.283214707341173,-0.303141259068211,
1.68332504372461));
#6829=CARTESIAN_POINT('Ctrl Pts',(0.244262842368623,-0.335108247315849,
1.68958170688653));
#6830=CARTESIAN_POINT('Ctrl Pts',(0.178166559972324,-0.373243761060364,
1.69769003172132));
#6831=CARTESIAN_POINT('Ctrl Pts',(0.143648558862931,-0.387888272594439,
1.70107730356824));
#6832=CARTESIAN_POINT('Ctrl Pts',(0.0717778861362652,-0.407041111792943,
1.70562212620408));
#6833=CARTESIAN_POINT('Ctrl Pts',(0.0344244045173309,-0.411552957311693,
1.706752));
#6834=CARTESIAN_POINT('Ctrl Pts',(-0.0344244045173315,-0.411552957311693,
1.706752));
#6835=CARTESIAN_POINT('Ctrl Pts',(-0.0717778861362658,-0.407041111792943,
1.70562212620408));
#6836=CARTESIAN_POINT('Ctrl Pts',(-0.143648558862932,-0.387888272594439,
1.70107730356824));
#6837=CARTESIAN_POINT('Ctrl Pts',(-0.178166559972325,-0.373243761060364,
1.69769003172132));
#6838=CARTESIAN_POINT('Ctrl Pts',(-0.244262842368624,-0.335108247315849,
1.68958170688653));
#6839=CARTESIAN_POINT('Ctrl Pts',(-0.283214707341173,-0.303141259068212,
1.68332504372461));
#6840=CARTESIAN_POINT('Ctrl Pts',(-0.341837165343982,-0.236152929235937,
1.67246562047521));
#6841=CARTESIAN_POINT('Ctrl Pts',(-0.368536561654408,-0.192480977588835,
1.66658649961961));
#6842=CARTESIAN_POINT('Ctrl Pts',(-0.394174530911059,-0.123823518623745,
1.66063136041479));
#6843=CARTESIAN_POINT('Ctrl Pts',(-0.400393769631748,-0.101649918886749,
1.65912839404491));
#6844=CARTESIAN_POINT('Ctrl Pts',(-0.404717578595297,-0.0793800000000001,
1.65807299932179));
#6845=CARTESIAN_POINT('',(-0.886256117232624,-0.07938,1.45861320581289));
#6846=CARTESIAN_POINT('Origin',(0.,-0.07938,0.));
#6847=CARTESIAN_POINT('',(-1.45861320581289,-0.07938,0.886256117232623));
#6848=CARTESIAN_POINT('Ctrl Pts',(-0.886256117232623,-0.0793800000000001,
1.45861320581289));
#6849=CARTESIAN_POINT('Ctrl Pts',(-0.890059788636852,-0.101649918886749,
1.45630208793976));
#6850=CARTESIAN_POINT('Ctrl Pts',(-0.895520212222106,-0.123823518623745,
1.45296717977858));
#6851=CARTESIAN_POINT('Ctrl Pts',(-0.917859913453974,-0.192480977588835,
1.43904931717599));
#6852=CARTESIAN_POINT('Ctrl Pts',(-0.940896403863071,-0.236152929235937,
1.4243271592157));
#6853=CARTESIAN_POINT('Ctrl Pts',(-0.990027513266105,-0.303141259068211,
1.39055359345152));
#6854=CARTESIAN_POINT('Ctrl Pts',(-1.02199477007745,-0.335108247315848,
1.36743459453896));
#6855=CARTESIAN_POINT('Ctrl Pts',(-1.07446535104584,-0.373243761060364,
1.32643091652006));
#6856=CARTESIAN_POINT('Ctrl Pts',(-1.10126842659597,-0.387888272594439,
1.30441816675528));
#6857=CARTESIAN_POINT('Ctrl Pts',(-1.15530234155453,-0.407041111792943,
1.25681160160691));
#6858=CARTESIAN_POINT('Ctrl Pts',(-1.18251418313119,-0.411552957311693,
1.23119764287622));
#6859=CARTESIAN_POINT('Ctrl Pts',(-1.23119764287622,-0.411552957311693,
1.18251418313119));
#6860=CARTESIAN_POINT('Ctrl Pts',(-1.25681160160691,-0.407041111792943,
1.15530234155453));
#6861=CARTESIAN_POINT('Ctrl Pts',(-1.30441816675528,-0.387888272594439,
1.10126842659597));
#6862=CARTESIAN_POINT('Ctrl Pts',(-1.32643091652006,-0.373243761060365,
1.07446535104584));
#6863=CARTESIAN_POINT('Ctrl Pts',(-1.36743459453896,-0.335108247315849,
1.02199477007745));
#6864=CARTESIAN_POINT('Ctrl Pts',(-1.39055359345152,-0.303141259068212,
0.990027513266106));
#6865=CARTESIAN_POINT('Ctrl Pts',(-1.4243271592157,-0.236152929235938,0.940896403863071));
#6866=CARTESIAN_POINT('Ctrl Pts',(-1.43904931717599,-0.192480977588836,
0.917859913453974));
#6867=CARTESIAN_POINT('Ctrl Pts',(-1.45296717977858,-0.123823518623746,
0.895520212222106));
#6868=CARTESIAN_POINT('Ctrl Pts',(-1.45630208793976,-0.101649918886749,
0.890059788636852));
#6869=CARTESIAN_POINT('Ctrl Pts',(-1.45861320581289,-0.0793800000000001,
0.886256117232623));
#6870=CARTESIAN_POINT('',(-1.65807299932179,-0.07938,0.404717578595295));
#6871=CARTESIAN_POINT('Origin',(0.,-0.07938,0.));
#6872=CARTESIAN_POINT('',(-1.706752,-0.411552957311693,2.08591827245526E-16));
#6873=CARTESIAN_POINT('Ctrl Pts',(-1.65807299932179,-0.0793800000000001,
0.404717578595296));
#6874=CARTESIAN_POINT('Ctrl Pts',(-1.65912839404491,-0.101649918886749,
0.400393769631747));
#6875=CARTESIAN_POINT('Ctrl Pts',(-1.66063136041479,-0.123823518623745,
0.394174530911058));
#6876=CARTESIAN_POINT('Ctrl Pts',(-1.66658649961961,-0.192480977588835,
0.368536561654407));
#6877=CARTESIAN_POINT('Ctrl Pts',(-1.67246562047521,-0.236152929235937,
0.341837165343982));
#6878=CARTESIAN_POINT('Ctrl Pts',(-1.68332504372461,-0.303141259068211,
0.283214707341173));
#6879=CARTESIAN_POINT('Ctrl Pts',(-1.68958170688653,-0.335108247315848,
0.244262842368623));
#6880=CARTESIAN_POINT('Ctrl Pts',(-1.69769003172132,-0.373243761060364,
0.178166559972324));
#6881=CARTESIAN_POINT('Ctrl Pts',(-1.70107730356824,-0.387888272594439,
0.143648558862931));
#6882=CARTESIAN_POINT('Ctrl Pts',(-1.70562212620408,-0.407041111792943,
0.0717778861362656));
#6883=CARTESIAN_POINT('Ctrl Pts',(-1.706752,-0.411552957311693,0.0344244045173313));
#6884=CARTESIAN_POINT('Ctrl Pts',(-1.706752,-0.411552957311693,2.08166817117217E-16));
#6885=CARTESIAN_POINT('',(-1.706752,-0.47628,2.09016837373834E-16));
#6886=CARTESIAN_POINT('',(-1.706752,-0.27783,2.09016837373834E-16));
#6887=CARTESIAN_POINT('Origin',(0.,-0.47628,0.));
#6888=CARTESIAN_POINT('',(-1.65807299932179,-0.07938,-0.404717578595296));
#6889=CARTESIAN_POINT('Ctrl Pts',(-1.706752,-0.411552957311693,2.0122792321331E-16));
#6890=CARTESIAN_POINT('Ctrl Pts',(-1.706752,-0.411552957311693,-0.0344244045173309));
#6891=CARTESIAN_POINT('Ctrl Pts',(-1.70562212620408,-0.407041111792943,
-0.0717778861362652));
#6892=CARTESIAN_POINT('Ctrl Pts',(-1.70107730356824,-0.387888272594439,
-0.143648558862931));
#6893=CARTESIAN_POINT('Ctrl Pts',(-1.69769003172132,-0.373243761060365,
-0.178166559972324));
#6894=CARTESIAN_POINT('Ctrl Pts',(-1.68958170688653,-0.335108247315849,
-0.244262842368623));
#6895=CARTESIAN_POINT('Ctrl Pts',(-1.68332504372461,-0.303141259068212,
-0.283214707341173));
#6896=CARTESIAN_POINT('Ctrl Pts',(-1.67246562047521,-0.236152929235938,
-0.341837165343982));
#6897=CARTESIAN_POINT('Ctrl Pts',(-1.66658649961961,-0.192480977588836,
-0.368536561654407));
#6898=CARTESIAN_POINT('Ctrl Pts',(-1.66063136041479,-0.123823518623745,
-0.394174530911059));
#6899=CARTESIAN_POINT('Ctrl Pts',(-1.65912839404491,-0.101649918886749,
-0.400393769631748));
#6900=CARTESIAN_POINT('Ctrl Pts',(-1.65807299932179,-0.0793800000000001,
-0.404717578595296));
#6901=CARTESIAN_POINT('',(-1.45861320581289,-0.07938,-0.886256117232623));
#6902=CARTESIAN_POINT('Origin',(0.,-0.07938,0.));
#6903=CARTESIAN_POINT('',(-0.886256117232623,-0.07938,-1.45861320581289));
#6904=CARTESIAN_POINT('Ctrl Pts',(-1.45861320581289,-0.0793800000000001,
-0.886256117232623));
#6905=CARTESIAN_POINT('Ctrl Pts',(-1.45630208793976,-0.101649918886749,
-0.890059788636852));
#6906=CARTESIAN_POINT('Ctrl Pts',(-1.45296717977858,-0.123823518623745,
-0.895520212222106));
#6907=CARTESIAN_POINT('Ctrl Pts',(-1.43904931717599,-0.192480977588835,
-0.917859913453974));
#6908=CARTESIAN_POINT('Ctrl Pts',(-1.4243271592157,-0.236152929235937,-0.940896403863072));
#6909=CARTESIAN_POINT('Ctrl Pts',(-1.39055359345152,-0.303141259068212,
-0.990027513266106));
#6910=CARTESIAN_POINT('Ctrl Pts',(-1.36743459453896,-0.335108247315849,
-1.02199477007745));
#6911=CARTESIAN_POINT('Ctrl Pts',(-1.32643091652006,-0.373243761060364,
-1.07446535104584));
#6912=CARTESIAN_POINT('Ctrl Pts',(-1.30441816675528,-0.387888272594439,
-1.10126842659597));
#6913=CARTESIAN_POINT('Ctrl Pts',(-1.25681160160691,-0.407041111792943,
-1.15530234155453));
#6914=CARTESIAN_POINT('Ctrl Pts',(-1.23119764287622,-0.411552957311693,
-1.18251418313119));
#6915=CARTESIAN_POINT('Ctrl Pts',(-1.18251418313119,-0.411552957311693,
-1.23119764287622));
#6916=CARTESIAN_POINT('Ctrl Pts',(-1.15530234155453,-0.407041111792943,
-1.25681160160691));
#6917=CARTESIAN_POINT('Ctrl Pts',(-1.10126842659597,-0.387888272594439,
-1.30441816675528));
#6918=CARTESIAN_POINT('Ctrl Pts',(-1.07446535104584,-0.373243761060364,
-1.32643091652006));
#6919=CARTESIAN_POINT('Ctrl Pts',(-1.02199477007745,-0.335108247315848,
-1.36743459453896));
#6920=CARTESIAN_POINT('Ctrl Pts',(-0.990027513266105,-0.303141259068211,
-1.39055359345152));
#6921=CARTESIAN_POINT('Ctrl Pts',(-0.940896403863071,-0.236152929235936,
-1.42432715921571));
#6922=CARTESIAN_POINT('Ctrl Pts',(-0.917859913453974,-0.192480977588835,
-1.43904931717599));
#6923=CARTESIAN_POINT('Ctrl Pts',(-0.895520212222106,-0.123823518623745,
-1.45296717977858));
#6924=CARTESIAN_POINT('Ctrl Pts',(-0.890059788636851,-0.101649918886749,
-1.45630208793976));
#6925=CARTESIAN_POINT('Ctrl Pts',(-0.886256117232623,-0.0793800000000001,
-1.45861320581289));
#6926=CARTESIAN_POINT('',(-0.404717578595295,-0.07938,-1.65807299932179));
#6927=CARTESIAN_POINT('Origin',(0.,-0.07938,0.));
#6928=CARTESIAN_POINT('',(0.404717578595296,-0.07938,-1.65807299932179));
#6929=CARTESIAN_POINT('Ctrl Pts',(-0.404717578595296,-0.0793800000000001,
-1.65807299932179));
#6930=CARTESIAN_POINT('Ctrl Pts',(-0.400393769631747,-0.101649918886749,
-1.65912839404491));
#6931=CARTESIAN_POINT('Ctrl Pts',(-0.394174530911058,-0.123823518623746,
-1.66063136041479));
#6932=CARTESIAN_POINT('Ctrl Pts',(-0.368536561654407,-0.192480977588836,
-1.66658649961961));
#6933=CARTESIAN_POINT('Ctrl Pts',(-0.341837165343982,-0.236152929235938,
-1.67246562047521));
#6934=CARTESIAN_POINT('Ctrl Pts',(-0.283214707341173,-0.303141259068212,
-1.68332504372461));
#6935=CARTESIAN_POINT('Ctrl Pts',(-0.244262842368623,-0.335108247315849,
-1.68958170688653));
#6936=CARTESIAN_POINT('Ctrl Pts',(-0.178166559972324,-0.373243761060364,
-1.69769003172132));
#6937=CARTESIAN_POINT('Ctrl Pts',(-0.143648558862931,-0.387888272594439,
-1.70107730356824));
#6938=CARTESIAN_POINT('Ctrl Pts',(-0.0717778861362653,-0.407041111792943,
-1.70562212620408));
#6939=CARTESIAN_POINT('Ctrl Pts',(-0.034424404517331,-0.411552957311693,
-1.706752));
#6940=CARTESIAN_POINT('Ctrl Pts',(0.0344244045173312,-0.411552957311693,
-1.706752));
#6941=CARTESIAN_POINT('Ctrl Pts',(0.0717778861362655,-0.407041111792943,
-1.70562212620408));
#6942=CARTESIAN_POINT('Ctrl Pts',(0.143648558862931,-0.387888272594439,
-1.70107730356824));
#6943=CARTESIAN_POINT('Ctrl Pts',(0.178166559972324,-0.373243761060364,
-1.69769003172132));
#6944=CARTESIAN_POINT('Ctrl Pts',(0.244262842368623,-0.335108247315849,
-1.68958170688653));
#6945=CARTESIAN_POINT('Ctrl Pts',(0.283214707341173,-0.303141259068212,
-1.68332504372461));
#6946=CARTESIAN_POINT('Ctrl Pts',(0.341837165343982,-0.236152929235937,
-1.67246562047521));
#6947=CARTESIAN_POINT('Ctrl Pts',(0.368536561654407,-0.192480977588835,
-1.66658649961961));
#6948=CARTESIAN_POINT('Ctrl Pts',(0.394174530911059,-0.123823518623745,
-1.66063136041479));
#6949=CARTESIAN_POINT('Ctrl Pts',(0.400393769631748,-0.101649918886749,
-1.65912839404491));
#6950=CARTESIAN_POINT('Ctrl Pts',(0.404717578595296,-0.0793800000000001,
-1.65807299932179));
#6951=CARTESIAN_POINT('',(0.886256117232623,-0.07938,-1.45861320581289));
#6952=CARTESIAN_POINT('Origin',(0.,-0.07938,0.));
#6953=CARTESIAN_POINT('',(1.45861320581289,-0.07938,-0.886256117232623));
#6954=CARTESIAN_POINT('Ctrl Pts',(0.886256117232623,-0.0793800000000001,
-1.45861320581289));
#6955=CARTESIAN_POINT('Ctrl Pts',(0.890059788636852,-0.101649918886749,
-1.45630208793976));
#6956=CARTESIAN_POINT('Ctrl Pts',(0.895520212222106,-0.123823518623745,
-1.45296717977858));
#6957=CARTESIAN_POINT('Ctrl Pts',(0.917859913453974,-0.192480977588835,
-1.43904931717599));
#6958=CARTESIAN_POINT('Ctrl Pts',(0.940896403863072,-0.236152929235937,
-1.4243271592157));
#6959=CARTESIAN_POINT('Ctrl Pts',(0.990027513266106,-0.303141259068211,
-1.39055359345152));
#6960=CARTESIAN_POINT('Ctrl Pts',(1.02199477007745,-0.335108247315849,-1.36743459453896));
#6961=CARTESIAN_POINT('Ctrl Pts',(1.07446535104584,-0.373243761060364,-1.32643091652006));
#6962=CARTESIAN_POINT('Ctrl Pts',(1.10126842659597,-0.387888272594439,-1.30441816675528));
#6963=CARTESIAN_POINT('Ctrl Pts',(1.15530234155453,-0.407041111792943,-1.25681160160691));
#6964=CARTESIAN_POINT('Ctrl Pts',(1.18251418313119,-0.411552957311693,-1.23119764287622));
#6965=CARTESIAN_POINT('Ctrl Pts',(1.23119764287622,-0.411552957311693,-1.18251418313119));
#6966=CARTESIAN_POINT('Ctrl Pts',(1.25681160160691,-0.407041111792943,-1.15530234155453));
#6967=CARTESIAN_POINT('Ctrl Pts',(1.30441816675528,-0.387888272594439,-1.10126842659597));
#6968=CARTESIAN_POINT('Ctrl Pts',(1.32643091652006,-0.373243761060364,-1.07446535104584));
#6969=CARTESIAN_POINT('Ctrl Pts',(1.36743459453896,-0.335108247315849,-1.02199477007745));
#6970=CARTESIAN_POINT('Ctrl Pts',(1.39055359345152,-0.303141259068212,-0.990027513266105));
#6971=CARTESIAN_POINT('Ctrl Pts',(1.4243271592157,-0.236152929235937,-0.940896403863071));
#6972=CARTESIAN_POINT('Ctrl Pts',(1.43904931717599,-0.192480977588835,-0.917859913453974));
#6973=CARTESIAN_POINT('Ctrl Pts',(1.45296717977858,-0.123823518623745,-0.895520212222106));
#6974=CARTESIAN_POINT('Ctrl Pts',(1.45630208793976,-0.101649918886749,-0.890059788636852));
#6975=CARTESIAN_POINT('Ctrl Pts',(1.45861320581289,-0.0793800000000001,
-0.886256117232623));
#6976=CARTESIAN_POINT('',(1.65807299932179,-0.07938,-0.404717578595296));
#6977=CARTESIAN_POINT('Origin',(0.,-0.07938,0.));
#6978=CARTESIAN_POINT('',(1.65807299932179,-0.07938,0.404717578595296));
#6979=CARTESIAN_POINT('Ctrl Pts',(1.65807299932179,-0.0793800000000001,
-0.404717578595296));
#6980=CARTESIAN_POINT('Ctrl Pts',(1.65912839404491,-0.101649918886749,-0.400393769631747));
#6981=CARTESIAN_POINT('Ctrl Pts',(1.66063136041479,-0.123823518623745,-0.394174530911058));
#6982=CARTESIAN_POINT('Ctrl Pts',(1.66658649961961,-0.192480977588835,-0.368536561654407));
#6983=CARTESIAN_POINT('Ctrl Pts',(1.67246562047521,-0.236152929235937,-0.341837165343982));
#6984=CARTESIAN_POINT('Ctrl Pts',(1.68332504372461,-0.303141259068212,-0.283214707341173));
#6985=CARTESIAN_POINT('Ctrl Pts',(1.68958170688653,-0.335108247315849,-0.244262842368623));
#6986=CARTESIAN_POINT('Ctrl Pts',(1.69769003172132,-0.373243761060364,-0.178166559972324));
#6987=CARTESIAN_POINT('Ctrl Pts',(1.70107730356824,-0.387888272594439,-0.143648558862931));
#6988=CARTESIAN_POINT('Ctrl Pts',(1.70562212620408,-0.407041111792943,-0.0717778861362655));
#6989=CARTESIAN_POINT('Ctrl Pts',(1.706752,-0.411552957311693,-0.0344244045173312));
#6990=CARTESIAN_POINT('Ctrl Pts',(1.706752,-0.411552957311693,0.0344244045173312));
#6991=CARTESIAN_POINT('Ctrl Pts',(1.70562212620408,-0.407041111792943,0.0717778861362655));
#6992=CARTESIAN_POINT('Ctrl Pts',(1.70107730356824,-0.387888272594439,0.143648558862931));
#6993=CARTESIAN_POINT('Ctrl Pts',(1.69769003172132,-0.373243761060364,0.178166559972324));
#6994=CARTESIAN_POINT('Ctrl Pts',(1.68958170688653,-0.335108247315849,0.244262842368623));
#6995=CARTESIAN_POINT('Ctrl Pts',(1.68332504372461,-0.303141259068212,0.283214707341173));
#6996=CARTESIAN_POINT('Ctrl Pts',(1.67246562047521,-0.236152929235937,0.341837165343982));
#6997=CARTESIAN_POINT('Ctrl Pts',(1.66658649961961,-0.192480977588835,0.368536561654407));
#6998=CARTESIAN_POINT('Ctrl Pts',(1.66063136041479,-0.123823518623745,0.394174530911058));
#6999=CARTESIAN_POINT('Ctrl Pts',(1.65912839404491,-0.101649918886749,0.400393769631747));
#7000=CARTESIAN_POINT('Ctrl Pts',(1.65807299932179,-0.0793800000000001,
0.404717578595296));
#7001=CARTESIAN_POINT('Origin',(0.,-0.07938,0.));
#7002=CARTESIAN_POINT('Origin',(0.,-0.07938,0.));
#7003=CARTESIAN_POINT('',(0.397005914195118,-0.07938,1.59456899932179));
#7004=CARTESIAN_POINT('Origin',(0.,-0.07938,0.));
#7005=CARTESIAN_POINT('Origin',(-3.33066907387547E-16,-0.07938,1.675));
#7006=CARTESIAN_POINT('Origin',(-3.33066907387547E-16,0.,1.675));
#7007=CARTESIAN_POINT('',(-0.397005914195118,-0.07938,1.59456899932179));
#7008=CARTESIAN_POINT('Ctrl Pts',(-0.397005914195119,-0.0793800000000001,
1.59456899932179));
#7009=CARTESIAN_POINT('Ctrl Pts',(-0.3886265584581,-0.123401821157026,1.59665523941937));
#7010=CARTESIAN_POINT('Ctrl Pts',(-0.373030350867485,-0.166543350814306,
1.60050712143809));
#7011=CARTESIAN_POINT('Ctrl Pts',(-0.333298652394954,-0.237231147975234,
1.60919314384089));
#7012=CARTESIAN_POINT('Ctrl Pts',(-0.311480544243687,-0.266264900654909,
1.61365775139403));
#7013=CARTESIAN_POINT('Ctrl Pts',(-0.261368388670537,-0.317195968905306,
1.62252828437015));
#7014=CARTESIAN_POINT('Ctrl Pts',(-0.233069203882014,-0.33909093068465,
1.62691869420078));
#7015=CARTESIAN_POINT('Ctrl Pts',(-0.174042761838764,-0.373586846396559,
1.63426473152765));
#7016=CARTESIAN_POINT('Ctrl Pts',(-0.14036578147155,-0.388086240756494,
1.63761964365402));
#7017=CARTESIAN_POINT('Ctrl Pts',(-0.0701778381840615,-0.407068917407805,
1.64212536811722));
#7018=CARTESIAN_POINT('Ctrl Pts',(-0.0336652739555918,-0.411552957311693,
1.643248));
#7019=CARTESIAN_POINT('Ctrl Pts',(0.0336652739555913,-0.411552957311693,
1.643248));
#7020=CARTESIAN_POINT('Ctrl Pts',(0.070177838184061,-0.407068917407805,
1.64212536811722));
#7021=CARTESIAN_POINT('Ctrl Pts',(0.140365781471549,-0.388086240756494,
1.63761964365402));
#7022=CARTESIAN_POINT('Ctrl Pts',(0.174042761838763,-0.373586846396559,
1.63426473152765));
#7023=CARTESIAN_POINT('Ctrl Pts',(0.233069203882014,-0.33909093068465,1.62691869420078));
#7024=CARTESIAN_POINT('Ctrl Pts',(0.261368388670536,-0.317195968905306,
1.62252828437015));
#7025=CARTESIAN_POINT('Ctrl Pts',(0.311480544243686,-0.266264900654908,
1.61365775139403));
#7026=CARTESIAN_POINT('Ctrl Pts',(0.333298652394954,-0.237231147975234,
1.60919314384089));
#7027=CARTESIAN_POINT('Ctrl Pts',(0.373030350867484,-0.166543350814306,
1.60050712143809));
#7028=CARTESIAN_POINT('Ctrl Pts',(0.388626558458099,-0.123401821157026,
1.59665523941937));
#7029=CARTESIAN_POINT('Ctrl Pts',(0.397005914195118,-0.07938,1.59456899932179));
#7030=CARTESIAN_POINT('Origin',(-3.33066907387547E-16,-0.07938,1.675));
#7031=CARTESIAN_POINT('Origin',(0.,-0.07938,0.));
#7032=CARTESIAN_POINT('',(-0.846804978391754,-0.07938,1.40825612658882));
#7033=CARTESIAN_POINT('Origin',(0.,-0.07938,0.));
#7034=CARTESIAN_POINT('Origin',(-1.18440385848747,-0.07938,1.18440385848747));
#7035=CARTESIAN_POINT('Origin',(-1.18440385848747,0.,1.18440385848747));
#7036=CARTESIAN_POINT('',(-1.40825612658882,-0.07938,0.846804978391753));
#7037=CARTESIAN_POINT('Ctrl Pts',(-1.40825612658882,-0.0793800000000001,
0.846804978391753));
#7038=CARTESIAN_POINT('Ctrl Pts',(-1.40380622184538,-0.123401821157026,
0.854205272175555));
#7039=CARTESIAN_POINT('Ctrl Pts',(-1.39550172959303,-0.166543350814306,
0.867957148219442));
#7040=CARTESIAN_POINT('Ctrl Pts',(-1.3735491215176,-0.237231147975235,0.902193646979983));
#7041=CARTESIAN_POINT('Ctrl Pts',(-1.36127834356734,-0.266264900654909,
0.920778333482565));
#7042=CARTESIAN_POINT('Ctrl Pts',(-1.33211611256184,-0.317195968905306,
0.962485392528369));
#7043=CARTESIAN_POINT('Ctrl Pts',(-1.31521005565926,-0.339090930684651,
0.985600426557816));
#7044=CARTESIAN_POINT('Ctrl Pts',(-1.27866649102984,-0.373586846396559,
1.03253285680459));
#7045=CARTESIAN_POINT('Ctrl Pts',(-1.25722555095714,-0.388086240756494,
1.05871835910697));
#7046=CARTESIAN_POINT('Ctrl Pts',(-1.2107812086231,-0.407068917407805,1.11153475808518));
#7047=CARTESIAN_POINT('Ctrl Pts',(-1.18575674747573,-0.411552957311693,
1.13814686046673));
#7048=CARTESIAN_POINT('Ctrl Pts',(-1.13814686046673,-0.411552957311693,
1.18575674747573));
#7049=CARTESIAN_POINT('Ctrl Pts',(-1.11153475808518,-0.407068917407805,
1.2107812086231));
#7050=CARTESIAN_POINT('Ctrl Pts',(-1.05871835910697,-0.388086240756494,
1.25722555095714));
#7051=CARTESIAN_POINT('Ctrl Pts',(-1.03253285680459,-0.373586846396559,
1.27866649102984));
#7052=CARTESIAN_POINT('Ctrl Pts',(-0.985600426557816,-0.33909093068465,
1.31521005565926));
#7053=CARTESIAN_POINT('Ctrl Pts',(-0.962485392528369,-0.317195968905306,
1.33211611256184));
#7054=CARTESIAN_POINT('Ctrl Pts',(-0.920778333482565,-0.266264900654908,
1.36127834356734));
#7055=CARTESIAN_POINT('Ctrl Pts',(-0.902193646979983,-0.237231147975234,
1.3735491215176));
#7056=CARTESIAN_POINT('Ctrl Pts',(-0.867957148219442,-0.166543350814306,
1.39550172959303));
#7057=CARTESIAN_POINT('Ctrl Pts',(-0.854205272175555,-0.123401821157026,
1.40380622184538));
#7058=CARTESIAN_POINT('Ctrl Pts',(-0.846804978391753,-0.0793800000000001,
1.40825612658882));
#7059=CARTESIAN_POINT('Origin',(-1.18440385848747,-0.07938,1.18440385848747));
#7060=CARTESIAN_POINT('Origin',(0.,-0.07938,0.));
#7061=CARTESIAN_POINT('',(-1.59456899932179,-0.07938,0.397005914195118));
#7062=CARTESIAN_POINT('Origin',(0.,-0.07938,0.));
#7063=CARTESIAN_POINT('Origin',(-1.675,-0.07938,-2.22044604925031E-16));
#7064=CARTESIAN_POINT('Origin',(-1.675,0.,-2.22044604925031E-16));
#7065=CARTESIAN_POINT('',(-1.59456899932179,-0.07938,-0.397005914195118));
#7066=CARTESIAN_POINT('',(-1.643248,-0.411552957311693,3.47540551556327E-18));
#7067=CARTESIAN_POINT('Ctrl Pts',(-1.59456899932179,-0.0793800000000001,
-0.397005914195119));
#7068=CARTESIAN_POINT('Ctrl Pts',(-1.59665523941937,-0.123401821157026,
-0.388626558458099));
#7069=CARTESIAN_POINT('Ctrl Pts',(-1.60050712143809,-0.166543350814306,
-0.373030350867485));
#7070=CARTESIAN_POINT('Ctrl Pts',(-1.60919314384089,-0.237231147975234,
-0.333298652394954));
#7071=CARTESIAN_POINT('Ctrl Pts',(-1.61365775139403,-0.266264900654909,
-0.311480544243686));
#7072=CARTESIAN_POINT('Ctrl Pts',(-1.62252828437015,-0.317195968905306,
-0.261368388670537));
#7073=CARTESIAN_POINT('Ctrl Pts',(-1.62691869420078,-0.33909093068465,-0.233069203882014));
#7074=CARTESIAN_POINT('Ctrl Pts',(-1.63426473152765,-0.373586846396559,
-0.174042761838764));
#7075=CARTESIAN_POINT('Ctrl Pts',(-1.63761964365402,-0.388086240756494,
-0.140365781471549));
#7076=CARTESIAN_POINT('Ctrl Pts',(-1.64212536811722,-0.407068917407805,
-0.0701778381840614));
#7077=CARTESIAN_POINT('Ctrl Pts',(-1.643248,-0.411552957311693,-0.0336652739555917));
#7078=CARTESIAN_POINT('Ctrl Pts',(-1.643248,-0.411552957311693,-2.0122792321331E-16));
#7079=CARTESIAN_POINT('Origin',(-1.675,-0.07938,-2.22044604925031E-16));
#7080=CARTESIAN_POINT('Ctrl Pts',(-1.643248,-0.411552957311693,-1.94289029309402E-16));
#7081=CARTESIAN_POINT('Ctrl Pts',(-1.643248,-0.411552957311693,0.0336652739555913));
#7082=CARTESIAN_POINT('Ctrl Pts',(-1.64212536811722,-0.407068917407805,
0.0701778381840609));
#7083=CARTESIAN_POINT('Ctrl Pts',(-1.63761964365402,-0.388086240756494,
0.140365781471549));
#7084=CARTESIAN_POINT('Ctrl Pts',(-1.63426473152765,-0.373586846396559,
0.174042761838763));
#7085=CARTESIAN_POINT('Ctrl Pts',(-1.62691869420078,-0.33909093068465,0.233069203882014));
#7086=CARTESIAN_POINT('Ctrl Pts',(-1.62252828437015,-0.317195968905306,
0.261368388670536));
#7087=CARTESIAN_POINT('Ctrl Pts',(-1.61365775139403,-0.266264900654909,
0.311480544243686));
#7088=CARTESIAN_POINT('Ctrl Pts',(-1.60919314384089,-0.237231147975235,
0.333298652394954));
#7089=CARTESIAN_POINT('Ctrl Pts',(-1.60050712143809,-0.166543350814306,
0.373030350867484));
#7090=CARTESIAN_POINT('Ctrl Pts',(-1.59665523941937,-0.123401821157026,
0.388626558458099));
#7091=CARTESIAN_POINT('Ctrl Pts',(-1.59456899932179,-0.0793800000000001,
0.397005914195118));
#7092=CARTESIAN_POINT('Origin',(0.,-0.07938,0.));
#7093=CARTESIAN_POINT('',(-1.40825612658882,-0.07938,-0.846804978391753));
#7094=CARTESIAN_POINT('Origin',(0.,-0.07938,0.));
#7095=CARTESIAN_POINT('Origin',(-1.18440385848747,-0.07938,-1.18440385848747));
#7096=CARTESIAN_POINT('Origin',(-1.18440385848747,0.,-1.18440385848747));
#7097=CARTESIAN_POINT('',(-0.846804978391753,-0.07938,-1.40825612658882));
#7098=CARTESIAN_POINT('Ctrl Pts',(-0.846804978391753,-0.0793800000000001,
-1.40825612658882));
#7099=CARTESIAN_POINT('Ctrl Pts',(-0.854205272175555,-0.123401821157026,
-1.40380622184538));
#7100=CARTESIAN_POINT('Ctrl Pts',(-0.867957148219442,-0.166543350814306,
-1.39550172959303));
#7101=CARTESIAN_POINT('Ctrl Pts',(-0.902193646979982,-0.237231147975234,
-1.3735491215176));
#7102=CARTESIAN_POINT('Ctrl Pts',(-0.920778333482564,-0.266264900654908,
-1.36127834356734));
#7103=CARTESIAN_POINT('Ctrl Pts',(-0.962485392528368,-0.317195968905306,
-1.33211611256184));
#7104=CARTESIAN_POINT('Ctrl Pts',(-0.985600426557816,-0.33909093068465,
-1.31521005565926));
#7105=CARTESIAN_POINT('Ctrl Pts',(-1.03253285680459,-0.373586846396559,
-1.27866649102984));
#7106=CARTESIAN_POINT('Ctrl Pts',(-1.05871835910697,-0.388086240756494,
-1.25722555095714));
#7107=CARTESIAN_POINT('Ctrl Pts',(-1.11153475808518,-0.407068917407805,
-1.2107812086231));
#7108=CARTESIAN_POINT('Ctrl Pts',(-1.13814686046673,-0.411552957311693,
-1.18575674747573));
#7109=CARTESIAN_POINT('Ctrl Pts',(-1.18575674747573,-0.411552957311693,
-1.13814686046673));
#7110=CARTESIAN_POINT('Ctrl Pts',(-1.2107812086231,-0.407068917407805,-1.11153475808518));
#7111=CARTESIAN_POINT('Ctrl Pts',(-1.25722555095714,-0.388086240756494,
-1.05871835910697));
#7112=CARTESIAN_POINT('Ctrl Pts',(-1.27866649102984,-0.373586846396559,
-1.03253285680459));
#7113=CARTESIAN_POINT('Ctrl Pts',(-1.31521005565926,-0.33909093068465,-0.985600426557816));
#7114=CARTESIAN_POINT('Ctrl Pts',(-1.33211611256184,-0.317195968905306,
-0.962485392528369));
#7115=CARTESIAN_POINT('Ctrl Pts',(-1.36127834356734,-0.266264900654909,
-0.920778333482565));
#7116=CARTESIAN_POINT('Ctrl Pts',(-1.3735491215176,-0.237231147975234,-0.902193646979983));
#7117=CARTESIAN_POINT('Ctrl Pts',(-1.39550172959303,-0.166543350814306,
-0.867957148219442));
#7118=CARTESIAN_POINT('Ctrl Pts',(-1.40380622184538,-0.123401821157026,
-0.854205272175555));
#7119=CARTESIAN_POINT('Ctrl Pts',(-1.40825612658882,-0.07938,-0.846804978391753));
#7120=CARTESIAN_POINT('Origin',(-1.18440385848747,-0.07938,-1.18440385848747));
#7121=CARTESIAN_POINT('Origin',(0.,-0.07938,0.));
#7122=CARTESIAN_POINT('',(-0.397005914195118,-0.07938,-1.59456899932179));
#7123=CARTESIAN_POINT('Origin',(0.,-0.07938,0.));
#7124=CARTESIAN_POINT('Origin',(1.11022302462516E-16,-0.07938,-1.675));
#7125=CARTESIAN_POINT('Origin',(1.11022302462516E-16,0.,-1.675));
#7126=CARTESIAN_POINT('',(0.397005914195118,-0.07938,-1.59456899932179));
#7127=CARTESIAN_POINT('Ctrl Pts',(0.397005914195119,-0.0793800000000001,
-1.59456899932179));
#7128=CARTESIAN_POINT('Ctrl Pts',(0.388626558458099,-0.123401821157026,
-1.59665523941937));
#7129=CARTESIAN_POINT('Ctrl Pts',(0.373030350867485,-0.166543350814306,
-1.60050712143809));
#7130=CARTESIAN_POINT('Ctrl Pts',(0.333298652394954,-0.237231147975234,
-1.60919314384089));
#7131=CARTESIAN_POINT('Ctrl Pts',(0.311480544243686,-0.266264900654909,
-1.61365775139403));
#7132=CARTESIAN_POINT('Ctrl Pts',(0.261368388670537,-0.317195968905306,
-1.62252828437015));
#7133=CARTESIAN_POINT('Ctrl Pts',(0.233069203882014,-0.33909093068465,-1.62691869420078));
#7134=CARTESIAN_POINT('Ctrl Pts',(0.174042761838763,-0.373586846396559,
-1.63426473152765));
#7135=CARTESIAN_POINT('Ctrl Pts',(0.140365781471549,-0.388086240756494,
-1.63761964365402));
#7136=CARTESIAN_POINT('Ctrl Pts',(0.0701778381840612,-0.407068917407805,
-1.64212536811722));
#7137=CARTESIAN_POINT('Ctrl Pts',(0.0336652739555916,-0.411552957311693,
-1.643248));
#7138=CARTESIAN_POINT('Ctrl Pts',(-0.0336652739555915,-0.411552957311693,
-1.643248));
#7139=CARTESIAN_POINT('Ctrl Pts',(-0.0701778381840612,-0.407068917407805,
-1.64212536811722));
#7140=CARTESIAN_POINT('Ctrl Pts',(-0.140365781471549,-0.388086240756494,
-1.63761964365402));
#7141=CARTESIAN_POINT('Ctrl Pts',(-0.174042761838764,-0.373586846396559,
-1.63426473152765));
#7142=CARTESIAN_POINT('Ctrl Pts',(-0.233069203882014,-0.33909093068465,
-1.62691869420078));
#7143=CARTESIAN_POINT('Ctrl Pts',(-0.261368388670536,-0.317195968905306,
-1.62252828437015));
#7144=CARTESIAN_POINT('Ctrl Pts',(-0.311480544243686,-0.266264900654908,
-1.61365775139403));
#7145=CARTESIAN_POINT('Ctrl Pts',(-0.333298652394954,-0.237231147975234,
-1.60919314384089));
#7146=CARTESIAN_POINT('Ctrl Pts',(-0.373030350867485,-0.166543350814306,
-1.60050712143809));
#7147=CARTESIAN_POINT('Ctrl Pts',(-0.388626558458099,-0.123401821157026,
-1.59665523941937));
#7148=CARTESIAN_POINT('Ctrl Pts',(-0.397005914195118,-0.07938,-1.59456899932179));
#7149=CARTESIAN_POINT('Origin',(1.11022302462516E-16,-0.07938,-1.675));
#7150=CARTESIAN_POINT('Origin',(0.,-0.07938,0.));
#7151=CARTESIAN_POINT('',(0.846804978391753,-0.07938,-1.40825612658882));
#7152=CARTESIAN_POINT('Origin',(0.,-0.07938,0.));
#7153=CARTESIAN_POINT('Origin',(1.18440385848747,-0.07938,-1.18440385848747));
#7154=CARTESIAN_POINT('Origin',(1.18440385848747,0.,-1.18440385848747));
#7155=CARTESIAN_POINT('',(1.40825612658882,-0.07938,-0.846804978391753));
#7156=CARTESIAN_POINT('Ctrl Pts',(1.40825612658882,-0.0793800000000001,
-0.846804978391753));
#7157=CARTESIAN_POINT('Ctrl Pts',(1.40380622184538,-0.123401821157026,-0.854205272175555));
#7158=CARTESIAN_POINT('Ctrl Pts',(1.39550172959303,-0.166543350814306,-0.867957148219442));
#7159=CARTESIAN_POINT('Ctrl Pts',(1.3735491215176,-0.237231147975234,-0.902193646979983));
#7160=CARTESIAN_POINT('Ctrl Pts',(1.36127834356734,-0.266264900654908,-0.920778333482565));
#7161=CARTESIAN_POINT('Ctrl Pts',(1.33211611256184,-0.317195968905306,-0.962485392528369));
#7162=CARTESIAN_POINT('Ctrl Pts',(1.31521005565926,-0.33909093068465,-0.985600426557816));
#7163=CARTESIAN_POINT('Ctrl Pts',(1.27866649102984,-0.373586846396559,-1.03253285680459));
#7164=CARTESIAN_POINT('Ctrl Pts',(1.25722555095714,-0.388086240756494,-1.05871835910697));
#7165=CARTESIAN_POINT('Ctrl Pts',(1.2107812086231,-0.407068917407805,-1.11153475808518));
#7166=CARTESIAN_POINT('Ctrl Pts',(1.18575674747573,-0.411552957311693,-1.13814686046673));
#7167=CARTESIAN_POINT('Ctrl Pts',(1.13814686046673,-0.411552957311693,-1.18575674747573));
#7168=CARTESIAN_POINT('Ctrl Pts',(1.11153475808518,-0.407068917407805,-1.2107812086231));
#7169=CARTESIAN_POINT('Ctrl Pts',(1.05871835910697,-0.388086240756494,-1.25722555095714));
#7170=CARTESIAN_POINT('Ctrl Pts',(1.03253285680459,-0.373586846396559,-1.27866649102984));
#7171=CARTESIAN_POINT('Ctrl Pts',(0.985600426557816,-0.33909093068465,-1.31521005565926));
#7172=CARTESIAN_POINT('Ctrl Pts',(0.962485392528369,-0.317195968905306,
-1.33211611256184));
#7173=CARTESIAN_POINT('Ctrl Pts',(0.920778333482565,-0.266264900654909,
-1.36127834356734));
#7174=CARTESIAN_POINT('Ctrl Pts',(0.902193646979983,-0.237231147975234,
-1.3735491215176));
#7175=CARTESIAN_POINT('Ctrl Pts',(0.867957148219442,-0.166543350814306,
-1.39550172959303));
#7176=CARTESIAN_POINT('Ctrl Pts',(0.854205272175555,-0.123401821157026,
-1.40380622184538));
#7177=CARTESIAN_POINT('Ctrl Pts',(0.846804978391753,-0.0793800000000001,
-1.40825612658882));
#7178=CARTESIAN_POINT('Origin',(1.18440385848747,-0.07938,-1.18440385848747));
#7179=CARTESIAN_POINT('Origin',(0.,-0.27783,0.));
#7180=CARTESIAN_POINT('',(-1.643248,-0.47628,2.01239840340529E-16));
#7181=CARTESIAN_POINT('Origin',(0.,-0.47628,0.));
#7182=CARTESIAN_POINT('',(-1.643248,-0.27783,2.01239840340529E-16));
#7183=CARTESIAN_POINT('',(1.59456899932179,-0.07938,0.397005914195118));
#7184=CARTESIAN_POINT('Origin',(0.,-0.07938,0.));
#7185=CARTESIAN_POINT('',(1.59456899932179,-0.07938,-0.397005914195118));
#7186=CARTESIAN_POINT('Ctrl Pts',(1.59456899932179,-0.0793800000000001,
0.397005914195118));
#7187=CARTESIAN_POINT('Ctrl Pts',(1.59665523941937,-0.123401821157026,0.388626558458099));
#7188=CARTESIAN_POINT('Ctrl Pts',(1.60050712143809,-0.166543350814306,0.373030350867485));
#7189=CARTESIAN_POINT('Ctrl Pts',(1.60919314384089,-0.237231147975234,0.333298652394954));
#7190=CARTESIAN_POINT('Ctrl Pts',(1.61365775139403,-0.266264900654909,0.311480544243686));
#7191=CARTESIAN_POINT('Ctrl Pts',(1.62252828437015,-0.317195968905306,0.261368388670537));
#7192=CARTESIAN_POINT('Ctrl Pts',(1.62691869420078,-0.33909093068465,0.233069203882014));
#7193=CARTESIAN_POINT('Ctrl Pts',(1.63426473152765,-0.373586846396559,0.174042761838764));
#7194=CARTESIAN_POINT('Ctrl Pts',(1.63761964365402,-0.388086240756494,0.140365781471549));
#7195=CARTESIAN_POINT('Ctrl Pts',(1.64212536811722,-0.407068917407805,0.0701778381840612));
#7196=CARTESIAN_POINT('Ctrl Pts',(1.643248,-0.411552957311693,0.0336652739555916));
#7197=CARTESIAN_POINT('Ctrl Pts',(1.643248,-0.411552957311693,-0.0336652739555916));
#7198=CARTESIAN_POINT('Ctrl Pts',(1.64212536811722,-0.407068917407805,-0.0701778381840612));
#7199=CARTESIAN_POINT('Ctrl Pts',(1.63761964365402,-0.388086240756494,-0.140365781471549));
#7200=CARTESIAN_POINT('Ctrl Pts',(1.63426473152765,-0.373586846396559,-0.174042761838764));
#7201=CARTESIAN_POINT('Ctrl Pts',(1.62691869420078,-0.33909093068465,-0.233069203882014));
#7202=CARTESIAN_POINT('Ctrl Pts',(1.62252828437015,-0.317195968905306,-0.261368388670537));
#7203=CARTESIAN_POINT('Ctrl Pts',(1.61365775139403,-0.266264900654909,-0.311480544243686));
#7204=CARTESIAN_POINT('Ctrl Pts',(1.60919314384089,-0.237231147975234,-0.333298652394954));
#7205=CARTESIAN_POINT('Ctrl Pts',(1.60050712143809,-0.166543350814306,-0.373030350867485));
#7206=CARTESIAN_POINT('Ctrl Pts',(1.59665523941937,-0.123401821157026,-0.388626558458099));
#7207=CARTESIAN_POINT('Ctrl Pts',(1.59456899932179,-0.07938,-0.397005914195118));
#7208=CARTESIAN_POINT('Origin',(0.,-0.07938,0.));
#7209=CARTESIAN_POINT('Origin',(0.,-0.07938,0.));
#7210=CARTESIAN_POINT('Origin',(1.675,-0.07938,0.));
#7211=CARTESIAN_POINT('Origin',(1.675,0.,0.));
#7212=CARTESIAN_POINT('Origin',(1.675,-0.07938,0.));
#7213=CARTESIAN_POINT('Origin',(0.,-0.47628,0.));
#7214=CARTESIAN_POINT('Origin',(0.,-0.07938,0.));
#7215=CARTESIAN_POINT('',(0.,0.,0.));
#7216=CARTESIAN_POINT('Origin',(1.70469,0.695,0.));
#7217=CARTESIAN_POINT('',(-1.70469,0.695,-2.0876431520385E-16));
#7218=CARTESIAN_POINT('Origin',(0.,0.695,0.));
#7219=CARTESIAN_POINT('',(-1.65031,0.695,-2.02104685910087E-16));
#7220=CARTESIAN_POINT('Origin',(0.,0.695,0.));
#7221=CARTESIAN_POINT('Origin',(0.,0.6575,0.));
#7222=CARTESIAN_POINT('',(-1.70469,0.62,-2.0876431520385E-16));
#7223=CARTESIAN_POINT('Origin',(0.,0.62,0.));
#7224=CARTESIAN_POINT('',(-1.70469,0.6575,-2.0876431520385E-16));
#7225=CARTESIAN_POINT('Origin',(1.65031,0.62,0.));
#7226=CARTESIAN_POINT('',(-1.65031,0.62,-2.02104685910087E-16));
#7227=CARTESIAN_POINT('Origin',(0.,0.62,0.));
#7228=CARTESIAN_POINT('Origin',(0.,0.6575,0.));
#7229=CARTESIAN_POINT('',(-1.65031,0.6575,-2.02104685910087E-16));
#7230=CARTESIAN_POINT('Origin',(1.70469,-0.62,0.));
#7231=CARTESIAN_POINT('',(-1.70469,-0.62,-2.0876431520385E-16));
#7232=CARTESIAN_POINT('Origin',(0.,-0.62,0.));
#7233=CARTESIAN_POINT('',(-1.65031,-0.62,-2.02104685910087E-16));
#7234=CARTESIAN_POINT('Origin',(0.,-0.62,0.));
#7235=CARTESIAN_POINT('Origin',(0.,-0.6575,0.));
#7236=CARTESIAN_POINT('',(-1.70469,-0.695,-2.0876431520385E-16));
#7237=CARTESIAN_POINT('Origin',(0.,-0.695,0.));
#7238=CARTESIAN_POINT('',(-1.70469,-0.6575,-2.0876431520385E-16));
#7239=CARTESIAN_POINT('Origin',(1.65031,-0.695,0.));
#7240=CARTESIAN_POINT('',(-1.65031,-0.695,-2.02104685910087E-16));
#7241=CARTESIAN_POINT('Origin',(0.,-0.695,0.));
#7242=CARTESIAN_POINT('Origin',(0.,-0.6575,0.));
#7243=CARTESIAN_POINT('',(-1.65031,-0.6575,-2.02104685910087E-16));
#7244=CARTESIAN_POINT('',(0.,0.,0.));
#7245=CARTESIAN_POINT('',(0.,0.,0.));
#7246=CARTESIAN_POINT('',(0.,0.,0.));
#7247=CARTESIAN_POINT('',(0.,0.,0.));
#7248=CARTESIAN_POINT('',(0.,0.,0.));
#7249=CARTESIAN_POINT('',(0.,0.,0.));
#7250=CARTESIAN_POINT('Origin',(0.45,0.6,0.));
#7251=CARTESIAN_POINT('',(-0.45,0.6,-5.51091059616309E-17));
#7252=CARTESIAN_POINT('Origin',(0.,0.6,0.));
#7253=CARTESIAN_POINT('Origin',(0.,0.575,0.));
#7254=CARTESIAN_POINT('',(-0.5,0.55,-6.12323399573677E-17));
#7255=CARTESIAN_POINT('Origin',(0.,0.55,0.));
#7256=CARTESIAN_POINT('',(-0.475,0.575,-5.81707229594993E-17));
#7257=CARTESIAN_POINT('Origin',(0.,0.29,0.));
#7258=CARTESIAN_POINT('',(-0.5,0.0299999999999998,-6.12323399573677E-17));
#7259=CARTESIAN_POINT('Origin',(0.,0.0299999999999998,0.));
#7260=CARTESIAN_POINT('',(-0.5,0.29,-6.12323399573677E-17));
#7261=CARTESIAN_POINT('Origin',(0.,0.0150000000000001,0.));
#7262=CARTESIAN_POINT('',(-0.47,7.11236625150491E-17,-5.75583995599256E-17));
#7263=CARTESIAN_POINT('Origin',(0.,0.,0.));
#7264=CARTESIAN_POINT('',(-0.485,0.0150000000000001,-5.93953697586466E-17));
#7265=CARTESIAN_POINT('Origin',(0.32,0.,0.));
#7266=CARTESIAN_POINT('',(-0.32,-6.93889390390723E-18,-3.91886975727153E-17));
#7267=CARTESIAN_POINT('Origin',(0.,0.,0.));
#7268=CARTESIAN_POINT('Origin',(0.,-0.02,0.));
#7269=CARTESIAN_POINT('',(-0.2942,-0.0515999999999999,3.60291088309151E-17));
#7270=CARTESIAN_POINT('Origin',(0.,-0.0515999999999999,0.));
#7271=CARTESIAN_POINT('',(-0.31,-0.02,-3.7964050773568E-17));
#7272=CARTESIAN_POINT('Origin',(0.,-1.24,0.));
#7273=CARTESIAN_POINT('',(-0.2942,-2.4458,3.60291088309151E-17));
#7274=CARTESIAN_POINT('Origin',(0.,-2.4458,0.));
#7275=CARTESIAN_POINT('',(-0.2942,-1.24,-3.60291088309151E-17));
#7276=CARTESIAN_POINT('Origin',(0.,-2.47,0.));
#7277=CARTESIAN_POINT('',(-0.24,-2.5,-2.93915231795365E-17));
#7278=CARTESIAN_POINT('Origin',(0.,-2.5,0.));
#7279=CARTESIAN_POINT('',(-0.27,-2.47,-3.30654635769785E-17));
#7280=CARTESIAN_POINT('Origin',(0.,-2.5,0.));
#7281=CARTESIAN_POINT('Origin',(0.144337567297406,-0.6,-0.25));
#7282=CARTESIAN_POINT('',(0.288675134594813,-0.6,0.));
#7283=CARTESIAN_POINT('',(0.144337567297406,-0.6,-0.25));
#7284=CARTESIAN_POINT('',(0.288675134594813,-0.6,0.));
#7285=CARTESIAN_POINT('',(0.144337567297406,-0.96,-0.25));
#7286=CARTESIAN_POINT('',(0.144337567297406,-0.6,-0.25));
#7287=CARTESIAN_POINT('',(0.288675134594813,-0.96,0.));
#7288=CARTESIAN_POINT('',(0.288675134594813,-0.96,0.));
#7289=CARTESIAN_POINT('',(0.288675134594813,-0.6,0.));
#7290=CARTESIAN_POINT('Origin',(-0.144337567297406,-0.6,-0.25));
#7291=CARTESIAN_POINT('',(-0.144337567297406,-0.6,-0.25));
#7292=CARTESIAN_POINT('',(0.144337567297406,-0.6,-0.25));
#7293=CARTESIAN_POINT('',(-0.144337567297406,-0.96,-0.25));
#7294=CARTESIAN_POINT('',(-0.144337567297406,-0.6,-0.25));
#7295=CARTESIAN_POINT('',(0.144337567297406,-0.96,-0.25));
#7296=CARTESIAN_POINT('Origin',(-0.288675134594813,-0.6,-8.32667268468867E-17));
#7297=CARTESIAN_POINT('',(-0.288675134594813,-0.6,-3.53525079574969E-17));
#7298=CARTESIAN_POINT('',(-0.144337567297406,-0.6,-0.25));
#7299=CARTESIAN_POINT('',(-0.288675134594813,-0.96,-5.55111512312578E-17));
#7300=CARTESIAN_POINT('',(-0.288675134594813,-0.6,-3.53525079574969E-17));
#7301=CARTESIAN_POINT('',(-0.144337567297406,-0.96,-0.25));
#7302=CARTESIAN_POINT('Origin',(-0.144337567297407,-0.6,0.25));
#7303=CARTESIAN_POINT('',(-0.144337567297407,-0.6,0.25));
#7304=CARTESIAN_POINT('',(-0.288675134594813,-0.6,-3.53525079574969E-17));
#7305=CARTESIAN_POINT('',(-0.144337567297407,-0.96,0.25));
#7306=CARTESIAN_POINT('',(-0.144337567297407,-0.6,0.25));
#7307=CARTESIAN_POINT('',(-0.288675134594813,-0.96,-3.53525079574969E-17));
#7308=CARTESIAN_POINT('Origin',(0.144337567297406,-0.6,0.25));
#7309=CARTESIAN_POINT('',(0.144337567297406,-0.6,0.25));
#7310=CARTESIAN_POINT('',(-0.144337567297407,-0.6,0.25));
#7311=CARTESIAN_POINT('',(0.144337567297406,-0.96,0.25));
#7312=CARTESIAN_POINT('',(0.144337567297406,-0.6,0.25));
#7313=CARTESIAN_POINT('',(-0.144337567297407,-0.96,0.25));
#7314=CARTESIAN_POINT('Origin',(0.288675134594813,-0.6,0.));
#7315=CARTESIAN_POINT('',(0.144337567297406,-0.6,0.25));
#7316=CARTESIAN_POINT('',(0.144337567297406,-0.96,0.25));
#7317=CARTESIAN_POINT('Origin',(0.,-0.6,0.));
#7318=CARTESIAN_POINT('Origin',(0.,-0.96,0.));
#7319=CARTESIAN_POINT('',(0.,0.,0.));
#7320=CARTESIAN_POINT('Origin',(0.3,0.4,0.));
#7321=CARTESIAN_POINT('',(-0.3,0.4,-3.67394039744206E-17));
#7322=CARTESIAN_POINT('Origin',(0.,0.4,0.));
#7323=CARTESIAN_POINT('Origin',(0.,0.375,0.));
#7324=CARTESIAN_POINT('',(-0.35,0.35,-4.28626379701573E-17));
#7325=CARTESIAN_POINT('Origin',(0.,0.35,0.));
#7326=CARTESIAN_POINT('',(-0.325,0.375,-3.9801020972289E-17));
#7327=CARTESIAN_POINT('Origin',(0.,0.19,0.));
#7328=CARTESIAN_POINT('',(-0.35,0.03,-4.28626379701574E-17));
#7329=CARTESIAN_POINT('Origin',(0.,0.03,0.));
#7330=CARTESIAN_POINT('',(-0.35,0.19,-4.28626379701574E-17));
#7331=CARTESIAN_POINT('Origin',(0.,0.0149999999999999,0.));
#7332=CARTESIAN_POINT('',(-0.32,-3.29597460435593E-17,-3.91886975727153E-17));
#7333=CARTESIAN_POINT('Origin',(0.,0.,0.));
#7334=CARTESIAN_POINT('',(-0.335,0.0149999999999999,-4.10256677714363E-17));
#7335=CARTESIAN_POINT('Origin',(0.22,0.,0.));
#7336=CARTESIAN_POINT('',(-0.22,-6.93889390390723E-18,-2.69422295812418E-17));
#7337=CARTESIAN_POINT('Origin',(0.,0.,0.));
#7338=CARTESIAN_POINT('Origin',(0.,-0.02,0.));
#7339=CARTESIAN_POINT('',(-0.1954,-0.0492,2.39295984553393E-17));
#7340=CARTESIAN_POINT('Origin',(0.,-0.0492,0.));
#7341=CARTESIAN_POINT('',(-0.21,-0.02,-2.57175827820944E-17));
#7342=CARTESIAN_POINT('Origin',(0.,-0.8,0.));
#7343=CARTESIAN_POINT('',(-0.1954,-1.5646,2.39295984553393E-17));
#7344=CARTESIAN_POINT('Origin',(0.,-1.5646,0.));
#7345=CARTESIAN_POINT('',(-0.1954,-0.8,-2.39295984553393E-17));
#7346=CARTESIAN_POINT('Origin',(0.,-1.58,0.));
#7347=CARTESIAN_POINT('',(-0.16,-1.6,-1.95943487863577E-17));
#7348=CARTESIAN_POINT('Origin',(0.,-1.6,0.));
#7349=CARTESIAN_POINT('',(-0.18,-1.58,-2.20436423846524E-17));
#7350=CARTESIAN_POINT('Origin',(0.,-1.6,0.));
#7351=CARTESIAN_POINT('Origin',(0.0866025403784439,-0.4,-0.15));
#7352=CARTESIAN_POINT('',(0.173205080756888,-0.4,0.));
#7353=CARTESIAN_POINT('',(0.0866025403784439,-0.4,-0.15));
#7354=CARTESIAN_POINT('',(0.173205080756888,-0.4,0.));
#7355=CARTESIAN_POINT('',(0.0866025403784439,-0.64,-0.15));
#7356=CARTESIAN_POINT('',(0.0866025403784439,-0.4,-0.15));
#7357=CARTESIAN_POINT('',(0.173205080756888,-0.64,0.));
#7358=CARTESIAN_POINT('',(0.173205080756888,-0.64,0.));
#7359=CARTESIAN_POINT('',(0.173205080756888,-0.4,0.));
#7360=CARTESIAN_POINT('Origin',(-0.0866025403784438,-0.4,-0.15));
#7361=CARTESIAN_POINT('',(-0.0866025403784438,-0.4,-0.15));
#7362=CARTESIAN_POINT('',(0.0866025403784439,-0.4,-0.15));
#7363=CARTESIAN_POINT('',(-0.0866025403784438,-0.64,-0.15));
#7364=CARTESIAN_POINT('',(-0.0866025403784438,-0.4,-0.15));
#7365=CARTESIAN_POINT('',(0.0866025403784439,-0.64,-0.15));
#7366=CARTESIAN_POINT('Origin',(-0.173205080756888,-0.4,-2.77555756156289E-17));
#7367=CARTESIAN_POINT('',(-0.173205080756888,-0.4,-2.12115047744981E-17));
#7368=CARTESIAN_POINT('',(-0.0866025403784438,-0.4,-0.15));
#7369=CARTESIAN_POINT('',(-0.173205080756888,-0.64,-2.77555756156289E-17));
#7370=CARTESIAN_POINT('',(-0.173205080756888,-0.4,-2.12115047744981E-17));
#7371=CARTESIAN_POINT('',(-0.0866025403784438,-0.64,-0.15));
#7372=CARTESIAN_POINT('Origin',(-0.0866025403784439,-0.4,0.15));
#7373=CARTESIAN_POINT('',(-0.0866025403784439,-0.4,0.15));
#7374=CARTESIAN_POINT('',(-0.173205080756888,-0.4,-2.12115047744981E-17));
#7375=CARTESIAN_POINT('',(-0.0866025403784439,-0.64,0.15));
#7376=CARTESIAN_POINT('',(-0.0866025403784439,-0.4,0.15));
#7377=CARTESIAN_POINT('',(-0.173205080756888,-0.64,-2.12115047744981E-17));
#7378=CARTESIAN_POINT('Origin',(0.0866025403784439,-0.4,0.15));
#7379=CARTESIAN_POINT('',(0.0866025403784439,-0.4,0.15));
#7380=CARTESIAN_POINT('',(-0.0866025403784439,-0.4,0.15));
#7381=CARTESIAN_POINT('',(0.0866025403784439,-0.64,0.15));
#7382=CARTESIAN_POINT('',(0.0866025403784439,-0.4,0.15));
#7383=CARTESIAN_POINT('',(-0.0866025403784439,-0.64,0.15));
#7384=CARTESIAN_POINT('Origin',(0.173205080756888,-0.4,0.));
#7385=CARTESIAN_POINT('',(0.0866025403784439,-0.4,0.15));
#7386=CARTESIAN_POINT('',(0.0866025403784439,-0.64,0.15));
#7387=CARTESIAN_POINT('Origin',(0.,-0.4,-2.77555756156289E-17));
#7388=CARTESIAN_POINT('Origin',(0.,-0.64,-2.77555756156289E-17));
#7389=CARTESIAN_POINT('',(0.,0.,0.));
#7390=CARTESIAN_POINT('',(0.,0.,0.));
#7391=CARTESIAN_POINT('',(0.,0.,0.));
#7392=CARTESIAN_POINT('',(0.,0.,0.));
#7393=CARTESIAN_POINT('',(0.,0.,0.));
#7394=CARTESIAN_POINT('',(0.,0.,0.));
#7395=CARTESIAN_POINT('',(0.,0.,0.));
#7396=CARTESIAN_POINT('',(0.,0.,0.));
#7397=CARTESIAN_POINT('',(0.,1.,4.5));
#7398=CARTESIAN_POINT('',(-3.8,1.,2.5));
#7399=CARTESIAN_POINT('',(3.8,1.,2.5));
#7400=CARTESIAN_POINT('',(0.,5.,4.5));
#7401=CARTESIAN_POINT('',(-3.8,5.,2.5));
#7402=CARTESIAN_POINT('',(3.8,5.,2.5));
#7403=CARTESIAN_POINT('',(2.8,-0.4,4.5));
#7404=CARTESIAN_POINT('',(0.,-0.4,7.3));
#7405=CARTESIAN_POINT('',(-2.8,-0.4,4.5));
#7406=CARTESIAN_POINT('',(-4.44089209850063E-16,-0.4,1.7));
#7407=CARTESIAN_POINT('',(2.8,6.4,4.5));
#7408=CARTESIAN_POINT('',(4.44089209850063E-16,6.4,7.3));
#7409=CARTESIAN_POINT('',(-2.8,6.4,4.5));
#7410=CARTESIAN_POINT('',(-4.44089209850063E-16,6.4,1.7));
#7411=CARTESIAN_POINT('',(0.,0.,0.));
#7412=CARTESIAN_POINT('',(0.,0.,0.));
#7413=CARTESIAN_POINT('Origin',(-0.3,-3.2,3.4));
#7414=CARTESIAN_POINT('',(-0.3,-0.8,3.54606079858305));
#7415=CARTESIAN_POINT('',(-0.3,-3.2,3.54606079858305));
#7416=CARTESIAN_POINT('',(-0.3,-4.,3.54606079858305));
#7417=CARTESIAN_POINT('',(-0.3,-0.8,3.85));
#7418=CARTESIAN_POINT('',(-0.3,-0.8,3.85));
#7419=CARTESIAN_POINT('',(-0.3,-3.2,3.85));
#7420=CARTESIAN_POINT('',(-0.3,-3.2,3.85));
#7421=CARTESIAN_POINT('',(-0.3,-3.2,3.85));
#7422=CARTESIAN_POINT('Origin',(0.,-3.2,3.625));
#7423=CARTESIAN_POINT('',(0.3,-3.2,3.54606079858305));
#7424=CARTESIAN_POINT('Origin',(0.,-3.2,4.5));
#7425=CARTESIAN_POINT('',(0.3,-3.2,3.85));
#7426=CARTESIAN_POINT('',(0.3,-3.2,3.85));
#7427=CARTESIAN_POINT('',(0.3,-3.2,3.4));
#7428=CARTESIAN_POINT('Origin',(0.3,-3.2,3.85));
#7429=CARTESIAN_POINT('',(0.3,-0.8,3.54606079858305));
#7430=CARTESIAN_POINT('',(0.3,-4.,3.54606079858305));
#7431=CARTESIAN_POINT('',(0.3,-0.8,3.85));
#7432=CARTESIAN_POINT('',(0.3,-3.2,3.85));
#7433=CARTESIAN_POINT('',(0.3,-0.8,3.4));
#7434=CARTESIAN_POINT('Origin',(-0.3,-3.2,3.85));
#7435=CARTESIAN_POINT('',(0.3,-0.8,3.85));
#7436=CARTESIAN_POINT('Origin',(0.,-0.8,3.625));
#7437=CARTESIAN_POINT('Origin',(0.,-0.8,4.5));
#7438=CARTESIAN_POINT('Origin',(0.,0.3,4.5));
#7439=CARTESIAN_POINT('',(-1.2,0.3,4.5));
#7440=CARTESIAN_POINT('Origin',(0.,0.3,4.5));
#7441=CARTESIAN_POINT('',(-1.,0.3,4.5));
#7442=CARTESIAN_POINT('Origin',(0.,0.3,4.5));
#7443=CARTESIAN_POINT('Origin',(0.,0.,4.5));
#7444=CARTESIAN_POINT('',(-1.2,0.,4.5));
#7445=CARTESIAN_POINT('Origin',(0.,0.,4.5));
#7446=CARTESIAN_POINT('',(-1.,0.,4.5));
#7447=CARTESIAN_POINT('Origin',(0.,0.,4.5));
#7448=CARTESIAN_POINT('Origin',(0.,0.,4.5));
#7449=CARTESIAN_POINT('',(-1.2,0.,4.5));
#7450=CARTESIAN_POINT('Origin',(0.,-4.,4.5));
#7451=CARTESIAN_POINT('',(-1.,-4.,4.5));
#7452=CARTESIAN_POINT('',(-1.,-4.,4.5));
#7453=CARTESIAN_POINT('Origin',(0.,-4.,4.5));
#7454=CARTESIAN_POINT('Origin',(0.,-4.,4.5));
#7455=CARTESIAN_POINT('',(-1.,6.8,4.5));
#7456=CARTESIAN_POINT('Origin',(0.,6.8,4.5));
#7457=CARTESIAN_POINT('',(-1.,-4.,4.5));
#7458=CARTESIAN_POINT('Origin',(0.,6.8,4.5));
#7459=CARTESIAN_POINT('Origin',(0.,-4.,4.5));
#7460=CARTESIAN_POINT('',(0.,0.,0.));
#7461=CARTESIAN_POINT('Origin',(0.,5.7,4.5));
#7462=CARTESIAN_POINT('',(-1.01,6.,4.5));
#7463=CARTESIAN_POINT('Origin',(0.,6.,4.5));
#7464=CARTESIAN_POINT('',(-1.01,5.7,4.5));
#7465=CARTESIAN_POINT('',(-1.01,5.7,4.5));
#7466=CARTESIAN_POINT('Origin',(0.,5.7,4.5));
#7467=CARTESIAN_POINT('Origin',(0.,5.7,4.5));
#7468=CARTESIAN_POINT('',(-1.35,6.,4.5));
#7469=CARTESIAN_POINT('Origin',(0.,6.,4.5));
#7470=CARTESIAN_POINT('',(-1.35,5.7,4.5));
#7471=CARTESIAN_POINT('',(-1.35,5.7,4.5));
#7472=CARTESIAN_POINT('Origin',(0.,5.7,4.5));
#7473=CARTESIAN_POINT('Origin',(0.,6.,4.5));
#7474=CARTESIAN_POINT('Origin',(0.,5.7,4.5));
#7475=CARTESIAN_POINT('',(0.,0.,0.));
#7476=CARTESIAN_POINT('Origin',(0.,6.4,5.49));
#7477=CARTESIAN_POINT('',(0.172988438920061,6.28094119100209,5.49));
#7478=CARTESIAN_POINT('',(0.172988438920061,6.51905880899791,5.49));
#7479=CARTESIAN_POINT('',(0.172988438920061,6.,5.49));
#7480=CARTESIAN_POINT('Origin',(0.,6.4,5.49));
#7481=CARTESIAN_POINT('Origin',(0.,6.4,5.49));
#7482=CARTESIAN_POINT('',(-0.172988438920061,6.28094119100209,5.49));
#7483=CARTESIAN_POINT('Ctrl Pts',(-0.172988438920061,6.28094119100209,5.49));
#7484=CARTESIAN_POINT('Ctrl Pts',(-0.165594865311318,6.27019857760471,5.49129192197638));
#7485=CARTESIAN_POINT('Ctrl Pts',(-0.157297138725608,6.26031229062726,5.49265394943905));
#7486=CARTESIAN_POINT('Ctrl Pts',(-0.129892073845076,6.23290722574673,5.4967480843909));
#7487=CARTESIAN_POINT('Ctrl Pts',(-0.106330167759284,6.21675794366705,5.49969589327638));
#7488=CARTESIAN_POINT('Ctrl Pts',(-0.05461290463241,6.19530220603509,5.50385029472357));
#7489=CARTESIAN_POINT('Ctrl Pts',(-0.0264512308298516,6.19,5.505));
#7490=CARTESIAN_POINT('Ctrl Pts',(0.0264512308298515,6.19,5.505));
#7491=CARTESIAN_POINT('Ctrl Pts',(0.0546129046324099,6.19530220603509,5.50385029472357));
#7492=CARTESIAN_POINT('Ctrl Pts',(0.106330167759284,6.21675794366705,5.49969589327638));
#7493=CARTESIAN_POINT('Ctrl Pts',(0.129892073845076,6.23290722574673,5.4967480843909));
#7494=CARTESIAN_POINT('Ctrl Pts',(0.157297138725608,6.26031229062726,5.49265394943905));
#7495=CARTESIAN_POINT('Ctrl Pts',(0.165594865311318,6.27019857760471,5.49129192197638));
#7496=CARTESIAN_POINT('Ctrl Pts',(0.172988438920061,6.28094119100209,5.49));
#7497=CARTESIAN_POINT('',(-0.21,6.4,5.49));
#7498=CARTESIAN_POINT('Origin',(0.,6.4,5.49));
#7499=CARTESIAN_POINT('',(-0.21,6.4,5.98522725533839));
#7500=CARTESIAN_POINT('',(-0.21,6.4,5.49));
#7501=CARTESIAN_POINT('',(0.21,6.4,5.98522725533839));
#7502=CARTESIAN_POINT('Ctrl Pts',(0.21,6.4,5.98522725533839));
#7503=CARTESIAN_POINT('Ctrl Pts',(0.21,6.37359447307555,5.98522725533839));
#7504=CARTESIAN_POINT('Ctrl Pts',(0.204715737269596,6.34545292590929,5.98600415954412));
#7505=CARTESIAN_POINT('Ctrl Pts',(0.183273763036332,6.29372373109487,5.98880073282317));
#7506=CARTESIAN_POINT('Ctrl Pts',(0.167117923970394,6.27013307587204,5.99077897157582));
#7507=CARTESIAN_POINT('Ctrl Pts',(0.129867169887369,6.23288232178902,5.99448481141327));
#7508=CARTESIAN_POINT('Ctrl Pts',(0.106276408305765,6.21672628999865,5.99645455657129));
#7509=CARTESIAN_POINT('Ctrl Pts',(0.0545468514059002,6.19528417517378,5.99923165515646));
#7510=CARTESIAN_POINT('Ctrl Pts',(0.0264051785092814,6.19,6.));
#7511=CARTESIAN_POINT('Ctrl Pts',(-0.0264051785092814,6.19,6.));
#7512=CARTESIAN_POINT('Ctrl Pts',(-0.0545468514059002,6.19528417517378,
5.99923165515646));
#7513=CARTESIAN_POINT('Ctrl Pts',(-0.106276408305765,6.21672628999865,5.99645455657129));
#7514=CARTESIAN_POINT('Ctrl Pts',(-0.129867169887369,6.23288232178902,5.99448481141327));
#7515=CARTESIAN_POINT('Ctrl Pts',(-0.167117923970394,6.27013307587204,5.99077897157582));
#7516=CARTESIAN_POINT('Ctrl Pts',(-0.183273763036332,6.29372373109487,5.98880073282317));
#7517=CARTESIAN_POINT('Ctrl Pts',(-0.204715737269596,6.34545292590929,5.98600415954412));
#7518=CARTESIAN_POINT('Ctrl Pts',(-0.21,6.37359447307555,5.98522725533839));
#7519=CARTESIAN_POINT('Ctrl Pts',(-0.21,6.4,5.98522725533839));
#7520=CARTESIAN_POINT('Ctrl Pts',(-0.21,6.4,5.98522725533839));
#7521=CARTESIAN_POINT('Ctrl Pts',(-0.21,6.42640552692446,5.98522725533839));
#7522=CARTESIAN_POINT('Ctrl Pts',(-0.204715737269596,6.45454707409071,5.98600415954412));
#7523=CARTESIAN_POINT('Ctrl Pts',(-0.183273763036332,6.50627626890513,5.98880073282317));
#7524=CARTESIAN_POINT('Ctrl Pts',(-0.167117923970394,6.52986692412796,5.99077897157582));
#7525=CARTESIAN_POINT('Ctrl Pts',(-0.129867169887369,6.56711767821098,5.99448481141327));
#7526=CARTESIAN_POINT('Ctrl Pts',(-0.106276408305765,6.58327371000135,5.99645455657129));
#7527=CARTESIAN_POINT('Ctrl Pts',(-0.0545468514059003,6.60471582482622,
5.99923165515646));
#7528=CARTESIAN_POINT('Ctrl Pts',(-0.0264051785092815,6.61,6.));
#7529=CARTESIAN_POINT('Ctrl Pts',(0.0264051785092814,6.61,6.));
#7530=CARTESIAN_POINT('Ctrl Pts',(0.0545468514059006,6.60471582482622,5.99923165515646));
#7531=CARTESIAN_POINT('Ctrl Pts',(0.106276408305766,6.58327371000135,5.99645455657129));
#7532=CARTESIAN_POINT('Ctrl Pts',(0.129867169887369,6.56711767821098,5.99448481141327));
#7533=CARTESIAN_POINT('Ctrl Pts',(0.167117923970393,6.52986692412796,5.99077897157582));
#7534=CARTESIAN_POINT('Ctrl Pts',(0.183273763036332,6.50627626890513,5.98880073282317));
#7535=CARTESIAN_POINT('Ctrl Pts',(0.204715737269596,6.45454707409071,5.98600415954412));
#7536=CARTESIAN_POINT('Ctrl Pts',(0.21,6.42640552692446,5.98522725533839));
#7537=CARTESIAN_POINT('Ctrl Pts',(0.21,6.4,5.98522725533839));
#7538=CARTESIAN_POINT('',(-0.172988438920061,6.51905880899791,5.49));
#7539=CARTESIAN_POINT('Origin',(0.,6.4,5.49));
#7540=CARTESIAN_POINT('Ctrl Pts',(0.172988438920061,6.51905880899791,5.49));
#7541=CARTESIAN_POINT('Ctrl Pts',(0.165594865311319,6.52980142239529,5.49129192197638));
#7542=CARTESIAN_POINT('Ctrl Pts',(0.157297138725609,6.53968770937274,5.49265394943905));
#7543=CARTESIAN_POINT('Ctrl Pts',(0.129892073845076,6.56709277425327,5.4967480843909));
#7544=CARTESIAN_POINT('Ctrl Pts',(0.106330167759284,6.58324205633295,5.49969589327638));
#7545=CARTESIAN_POINT('Ctrl Pts',(0.05461290463241,6.60469779396491,5.50385029472357));
#7546=CARTESIAN_POINT('Ctrl Pts',(0.0264512308298516,6.61,5.505));
#7547=CARTESIAN_POINT('Ctrl Pts',(-0.0264512308298515,6.61,5.505));
#7548=CARTESIAN_POINT('Ctrl Pts',(-0.05461290463241,6.60469779396491,5.50385029472357));
#7549=CARTESIAN_POINT('Ctrl Pts',(-0.106330167759284,6.58324205633295,5.49969589327638));
#7550=CARTESIAN_POINT('Ctrl Pts',(-0.129892073845076,6.56709277425328,5.4967480843909));
#7551=CARTESIAN_POINT('Ctrl Pts',(-0.157297138725609,6.53968770937274,5.49265394943905));
#7552=CARTESIAN_POINT('Ctrl Pts',(-0.165594865311318,6.52980142239529,5.49129192197638));
#7553=CARTESIAN_POINT('Ctrl Pts',(-0.172988438920062,6.51905880899791,5.49));
#7554=CARTESIAN_POINT('Origin',(0.,6.4,5.49));
#7555=CARTESIAN_POINT('',(-0.172988438920061,6.,5.49));
#7556=CARTESIAN_POINT('Origin',(0.,6.,4.5));
#7557=CARTESIAN_POINT('',(-1.005,6.8,4.5));
#7558=CARTESIAN_POINT('Origin',(0.,6.8,4.5));
#7559=CARTESIAN_POINT('',(-1.005,6.,4.5));
#7560=CARTESIAN_POINT('',(-1.005,6.,4.5));
#7561=CARTESIAN_POINT('Origin',(0.,6.,4.5));
#7562=CARTESIAN_POINT('Origin',(0.,6.,4.5));
#7563=CARTESIAN_POINT('',(-1.5,6.8,4.5));
#7564=CARTESIAN_POINT('Origin',(0.,6.8,4.5));
#7565=CARTESIAN_POINT('',(-1.5,6.,4.5));
#7566=CARTESIAN_POINT('',(-1.5,6.,4.5));
#7567=CARTESIAN_POINT('Origin',(0.,6.,4.5));
#7568=CARTESIAN_POINT('Origin',(0.,6.8,4.5));
#7569=CARTESIAN_POINT('Origin',(0.,6.,4.5));
#7570=CARTESIAN_POINT('',(0.,0.,0.));
#7571=CARTESIAN_POINT('Origin',(0.,-1.2,5.49));
#7572=CARTESIAN_POINT('',(0.141067359796657,-1.35556349186104,5.49));
#7573=CARTESIAN_POINT('',(0.141067359796657,-1.04443650813896,5.49));
#7574=CARTESIAN_POINT('',(0.141067359796657,-3.5,5.49));
#7575=CARTESIAN_POINT('Origin',(0.,-1.2,5.49));
#7576=CARTESIAN_POINT('Origin',(0.,-1.2,5.49));
#7577=CARTESIAN_POINT('',(-0.141067359796657,-1.35556349186104,5.49));
#7578=CARTESIAN_POINT('Ctrl Pts',(-0.141067359796657,-1.35556349186104,
5.49));
#7579=CARTESIAN_POINT('Ctrl Pts',(-0.123818356698224,-1.3712051523632,5.49245784982446));
#7580=CARTESIAN_POINT('Ctrl Pts',(-0.102998643109699,-1.38462404333102,
5.49493819304946));
#7581=CARTESIAN_POINT('Ctrl Pts',(-0.054614114398353,-1.40469746372443,
5.49884449237241));
#7582=CARTESIAN_POINT('Ctrl Pts',(-0.0264520736824499,-1.41,5.5));
#7583=CARTESIAN_POINT('Ctrl Pts',(0.0264520736824498,-1.41,5.5));
#7584=CARTESIAN_POINT('Ctrl Pts',(0.0546141143983528,-1.40469746372443,
5.49884449237241));
#7585=CARTESIAN_POINT('Ctrl Pts',(0.102998643109699,-1.38462404333102,5.49493819304946));
#7586=CARTESIAN_POINT('Ctrl Pts',(0.123818356698224,-1.3712051523632,5.49245784982446));
#7587=CARTESIAN_POINT('Ctrl Pts',(0.141067359796657,-1.35556349186104,5.49));
#7588=CARTESIAN_POINT('',(-0.21,-1.2,5.49));
#7589=CARTESIAN_POINT('Origin',(0.,-1.2,5.49));
#7590=CARTESIAN_POINT('',(-0.21,-1.2,6.08615888233178));
#7591=CARTESIAN_POINT('',(-0.21,-1.2,5.49));
#7592=CARTESIAN_POINT('',(0.21,-1.2,6.08615888233178));
#7593=CARTESIAN_POINT('Ctrl Pts',(0.21,-1.2,6.08615888233178));
#7594=CARTESIAN_POINT('Ctrl Pts',(0.21,-1.22640093420375,6.08615888233178));
#7595=CARTESIAN_POINT('Ctrl Pts',(0.20471752266132,-1.25454055536511,6.08688606295397));
#7596=CARTESIAN_POINT('Ctrl Pts',(0.183276841782292,-1.3062710523005,6.08950502964782));
#7597=CARTESIAN_POINT('Ctrl Pts',(0.167120287247804,-1.32986456085055,6.09135816887013));
#7598=CARTESIAN_POINT('Ctrl Pts',(0.129864750292352,-1.367120097806,6.09483075953278));
#7599=CARTESIAN_POINT('Ctrl Pts',(0.106271159541076,-1.38327680083123,6.09667690933009));
#7600=CARTESIAN_POINT('Ctrl Pts',(0.0545403836274685,-1.4047175903444,6.09927985626981));
#7601=CARTESIAN_POINT('Ctrl Pts',(0.0264006657112964,-1.41,6.1));
#7602=CARTESIAN_POINT('Ctrl Pts',(-0.0264006657112964,-1.41,6.1));
#7603=CARTESIAN_POINT('Ctrl Pts',(-0.0545403836274684,-1.4047175903444,
6.09927985626981));
#7604=CARTESIAN_POINT('Ctrl Pts',(-0.106271159541075,-1.38327680083123,
6.09667690933009));
#7605=CARTESIAN_POINT('Ctrl Pts',(-0.129864750292352,-1.367120097806,6.09483075953278));
#7606=CARTESIAN_POINT('Ctrl Pts',(-0.167120287247804,-1.32986456085055,
6.09135816887013));
#7607=CARTESIAN_POINT('Ctrl Pts',(-0.183276841782292,-1.3062710523005,6.08950502964782));
#7608=CARTESIAN_POINT('Ctrl Pts',(-0.20471752266132,-1.25454055536511,6.08688606295397));
#7609=CARTESIAN_POINT('Ctrl Pts',(-0.21,-1.22640093420375,6.08615888233178));
#7610=CARTESIAN_POINT('Ctrl Pts',(-0.21,-1.2,6.08615888233178));
#7611=CARTESIAN_POINT('Ctrl Pts',(-0.21,-1.2,6.08615888233178));
#7612=CARTESIAN_POINT('Ctrl Pts',(-0.21,-1.17359906579625,6.08615888233178));
#7613=CARTESIAN_POINT('Ctrl Pts',(-0.20471752266132,-1.14545944463489,6.08688606295397));
#7614=CARTESIAN_POINT('Ctrl Pts',(-0.183276841782292,-1.0937289476995,6.08950502964782));
#7615=CARTESIAN_POINT('Ctrl Pts',(-0.167120287247804,-1.07013543914945,
6.09135816887013));
#7616=CARTESIAN_POINT('Ctrl Pts',(-0.129864750292352,-1.032879902194,6.09483075953278));
#7617=CARTESIAN_POINT('Ctrl Pts',(-0.106271159541076,-1.01672319916877,
6.09667690933009));
#7618=CARTESIAN_POINT('Ctrl Pts',(-0.0545403836274687,-0.995282409655599,
6.09927985626981));
#7619=CARTESIAN_POINT('Ctrl Pts',(-0.0264006657112964,-0.99,6.1));
#7620=CARTESIAN_POINT('Ctrl Pts',(0.0264006657112964,-0.99,6.1));
#7621=CARTESIAN_POINT('Ctrl Pts',(0.0545403836274687,-0.995282409655599,
6.09927985626981));
#7622=CARTESIAN_POINT('Ctrl Pts',(0.106271159541076,-1.01672319916877,6.09667690933009));
#7623=CARTESIAN_POINT('Ctrl Pts',(0.129864750292352,-1.032879902194,6.09483075953278));
#7624=CARTESIAN_POINT('Ctrl Pts',(0.167120287247804,-1.07013543914945,6.09135816887013));
#7625=CARTESIAN_POINT('Ctrl Pts',(0.183276841782292,-1.0937289476995,6.08950502964782));
#7626=CARTESIAN_POINT('Ctrl Pts',(0.20471752266132,-1.14545944463489,6.08688606295397));
#7627=CARTESIAN_POINT('Ctrl Pts',(0.21,-1.17359906579625,6.08615888233178));
#7628=CARTESIAN_POINT('Ctrl Pts',(0.21,-1.2,6.08615888233178));
#7629=CARTESIAN_POINT('',(-0.141067359796657,-1.04443650813896,5.49));
#7630=CARTESIAN_POINT('Origin',(0.,-1.2,5.49));
#7631=CARTESIAN_POINT('Ctrl Pts',(0.141067359796657,-1.04443650813896,5.49));
#7632=CARTESIAN_POINT('Ctrl Pts',(0.123818356698224,-1.0287948476368,5.49245784982446));
#7633=CARTESIAN_POINT('Ctrl Pts',(0.102998643109699,-1.01537595666898,5.49493819304946));
#7634=CARTESIAN_POINT('Ctrl Pts',(0.0546141143983531,-0.995302536275572,
5.49884449237241));
#7635=CARTESIAN_POINT('Ctrl Pts',(0.0264520736824498,-0.99,5.5));
#7636=CARTESIAN_POINT('Ctrl Pts',(-0.0264520736824498,-0.99,5.5));
#7637=CARTESIAN_POINT('Ctrl Pts',(-0.054614114398353,-0.995302536275572,
5.49884449237241));
#7638=CARTESIAN_POINT('Ctrl Pts',(-0.102998643109699,-1.01537595666898,
5.49493819304946));
#7639=CARTESIAN_POINT('Ctrl Pts',(-0.123818356698224,-1.0287948476368,5.49245784982446));
#7640=CARTESIAN_POINT('Ctrl Pts',(-0.141067359796657,-1.04443650813896,
5.49));
#7641=CARTESIAN_POINT('Origin',(0.,-1.2,5.49));
#7642=CARTESIAN_POINT('',(-0.141067359796657,-3.5,5.49));
#7643=CARTESIAN_POINT('Origin',(-0.3,-3.6,3.22));
#7644=CARTESIAN_POINT('',(-0.3,-3.5,3.22));
#7645=CARTESIAN_POINT('',(-0.3,-3.5,3.54606079858305));
#7646=CARTESIAN_POINT('',(-0.3,-3.5,3.86));
#7647=CARTESIAN_POINT('',(-0.3,-0.5,3.22));
#7648=CARTESIAN_POINT('',(-0.3,-3.6,3.22));
#7649=CARTESIAN_POINT('',(-0.3,-0.5,3.54606079858305));
#7650=CARTESIAN_POINT('',(-0.3,-0.5,3.86));
#7651=CARTESIAN_POINT('',(-0.3,-3.5,3.54606079858305));
#7652=CARTESIAN_POINT('Origin',(0.3,-3.6,3.22));
#7653=CARTESIAN_POINT('',(0.3,-3.5,3.22));
#7654=CARTESIAN_POINT('',(0.15,-3.5,3.22));
#7655=CARTESIAN_POINT('',(0.3,-0.5,3.22));
#7656=CARTESIAN_POINT('',(0.3,-3.6,3.22));
#7657=CARTESIAN_POINT('',(0.15,-0.5,3.22));
#7658=CARTESIAN_POINT('Origin',(0.3,-3.6,4.5));
#7659=CARTESIAN_POINT('',(0.3,-3.5,3.54606079858305));
#7660=CARTESIAN_POINT('',(0.3,-3.5,4.5));
#7661=CARTESIAN_POINT('',(0.3,-0.5,3.54606079858305));
#7662=CARTESIAN_POINT('',(0.3,-3.5,3.54606079858305));
#7663=CARTESIAN_POINT('',(0.3,-0.5,4.5));
#7664=CARTESIAN_POINT('Origin',(0.,-0.5,4.5));
#7665=CARTESIAN_POINT('',(-1.6,-0.5,4.5));
#7666=CARTESIAN_POINT('Origin',(0.,-0.5,4.5));
#7667=CARTESIAN_POINT('Origin',(0.,-0.5,4.5));
#7668=CARTESIAN_POINT('Origin',(0.,-3.5,4.5));
#7669=CARTESIAN_POINT('Origin',(0.,-3.5,4.5));
#7670=CARTESIAN_POINT('Origin',(-2.5,-3.6,4.5));
#7671=CARTESIAN_POINT('',(-2.83,-3.5,4.5));
#7672=CARTESIAN_POINT('Origin',(-2.5,-3.5,4.5));
#7673=CARTESIAN_POINT('',(-2.83,-2.9,4.5));
#7674=CARTESIAN_POINT('',(-2.83,-3.6,4.5));
#7675=CARTESIAN_POINT('Origin',(-2.5,-2.9,4.5));
#7676=CARTESIAN_POINT('Origin',(1.53080849893419E-16,-3.6,7.));
#7677=CARTESIAN_POINT('',(-0.33,-3.5,7.));
#7678=CARTESIAN_POINT('Origin',(1.53080849893419E-16,-3.5,7.));
#7679=CARTESIAN_POINT('',(-0.33,-2.9,7.));
#7680=CARTESIAN_POINT('',(-0.33,-3.6,7.));
#7681=CARTESIAN_POINT('Origin',(1.53080849893419E-16,-2.9,7.));
#7682=CARTESIAN_POINT('Origin',(2.5,-3.6,4.5));
#7683=CARTESIAN_POINT('',(2.17,-3.5,4.5));
#7684=CARTESIAN_POINT('Origin',(2.5,-3.5,4.5));
#7685=CARTESIAN_POINT('',(2.17,-2.9,4.5));
#7686=CARTESIAN_POINT('',(2.17,-3.6,4.5));
#7687=CARTESIAN_POINT('Origin',(2.5,-2.9,4.5));
#7688=CARTESIAN_POINT('Origin',(-4.59242549680257E-16,-3.6,2.));
#7689=CARTESIAN_POINT('',(-0.33,-3.5,2.));
#7690=CARTESIAN_POINT('Origin',(-4.59242549680257E-16,-3.5,2.));
#7691=CARTESIAN_POINT('',(-0.33,-2.9,2.));
#7692=CARTESIAN_POINT('',(-0.33,-3.6,2.));
#7693=CARTESIAN_POINT('Origin',(-4.59242549680257E-16,-2.9,2.));
#7694=CARTESIAN_POINT('Origin',(0.,-2.9,4.5));
#7695=CARTESIAN_POINT('',(-3.5,-2.9,4.5));
#7696=CARTESIAN_POINT('Origin',(0.,-2.9,4.5));
#7697=CARTESIAN_POINT('',(-1.6,-2.9,4.5));
#7698=CARTESIAN_POINT('Origin',(0.,-2.9,4.5));
#7699=CARTESIAN_POINT('Origin',(0.,-3.5,4.5));
#7700=CARTESIAN_POINT('',(-3.5,-3.5,4.5));
#7701=CARTESIAN_POINT('',(-3.5,-3.5,4.5));
#7702=CARTESIAN_POINT('Origin',(0.,-3.5,4.5));
#7703=CARTESIAN_POINT('Origin',(0.,-3.5,4.5));
#7704=CARTESIAN_POINT('',(-1.6,-3.5,4.5));
#7705=CARTESIAN_POINT('Origin',(0.,-3.5,4.5));
#7706=CARTESIAN_POINT('',(0.,0.,0.));
#7707=CARTESIAN_POINT('Origin',(-1.,0.,0.35));
#7708=CARTESIAN_POINT('',(-1.,-0.26,0.6));
#7709=CARTESIAN_POINT('',(-1.,-0.3,0.56));
#7710=CARTESIAN_POINT('',(-1.,-0.2675,0.5925));
#7711=CARTESIAN_POINT('',(-1.,0.26,0.6));
#7712=CARTESIAN_POINT('',(-1.,0.,0.6));
#7713=CARTESIAN_POINT('',(-1.,0.3,0.56));
#7714=CARTESIAN_POINT('',(-1.,0.2675,0.5925));
#7715=CARTESIAN_POINT('',(-1.,0.3,0.04));
#7716=CARTESIAN_POINT('',(-1.,0.3,0.175));
#7717=CARTESIAN_POINT('',(-1.,0.26,0.));
#7718=CARTESIAN_POINT('',(-1.,0.2925,0.0325));
#7719=CARTESIAN_POINT('',(-1.,-0.26,0.));
#7720=CARTESIAN_POINT('',(-1.,0.,0.));
#7721=CARTESIAN_POINT('',(-1.,-0.3,0.04));
#7722=CARTESIAN_POINT('',(-1.,-0.2925,0.0325));
#7723=CARTESIAN_POINT('',(-1.,-0.3,0.175));
#7724=CARTESIAN_POINT('Origin',(0.75,0.28,0.02));
#7725=CARTESIAN_POINT('',(1.,0.3,0.04));
#7726=CARTESIAN_POINT('',(0.75,0.3,0.04));
#7727=CARTESIAN_POINT('',(1.,0.26,0.));
#7728=CARTESIAN_POINT('',(1.,0.2925,0.0325));
#7729=CARTESIAN_POINT('',(0.75,0.26,0.));
#7730=CARTESIAN_POINT('Origin',(1.5,0.3,0.));
#7731=CARTESIAN_POINT('',(1.,0.3,0.56));
#7732=CARTESIAN_POINT('',(0.75,0.3,0.56));
#7733=CARTESIAN_POINT('',(1.,0.3,0.175));
#7734=CARTESIAN_POINT('Origin',(0.75,0.28,0.58));
#7735=CARTESIAN_POINT('',(1.,0.26,0.6));
#7736=CARTESIAN_POINT('',(0.75,0.26,0.6));
#7737=CARTESIAN_POINT('',(1.,0.2675,0.5925));
#7738=CARTESIAN_POINT('Origin',(0.,0.,0.6));
#7739=CARTESIAN_POINT('',(1.,-0.26,0.6));
#7740=CARTESIAN_POINT('',(-0.75,-0.26,0.6));
#7741=CARTESIAN_POINT('',(1.,0.,0.6));
#7742=CARTESIAN_POINT('Origin',(1.,0.,0.35));
#7743=CARTESIAN_POINT('',(1.,-0.26,0.));
#7744=CARTESIAN_POINT('',(1.,-0.3,0.04));
#7745=CARTESIAN_POINT('',(1.,-0.2925,0.0325));
#7746=CARTESIAN_POINT('',(1.,0.,0.));
#7747=CARTESIAN_POINT('',(1.,-0.3,0.56));
#7748=CARTESIAN_POINT('',(1.,-0.2675,0.5925));
#7749=CARTESIAN_POINT('',(1.,-0.3,0.175));
#7750=CARTESIAN_POINT('Origin',(0.,0.,0.));
#7751=CARTESIAN_POINT('',(-0.75,-0.26,0.));
#7752=CARTESIAN_POINT('Origin',(-0.75,-0.28,0.58));
#7753=CARTESIAN_POINT('',(-0.75,-0.3,0.56));
#7754=CARTESIAN_POINT('Origin',(-0.75,-0.28,0.02));
#7755=CARTESIAN_POINT('',(-0.75,-0.3,0.04));
#7756=CARTESIAN_POINT('Origin',(-1.5,-0.3,0.));
#7757=CARTESIAN_POINT('',(0.,0.,0.));
#7758=CARTESIAN_POINT('Origin',(0.0721687836487032,0.,-0.125));
#7759=CARTESIAN_POINT('',(0.0721687836487032,0.,-0.125));
#7760=CARTESIAN_POINT('',(0.144337567297406,0.,0.));
#7761=CARTESIAN_POINT('',(0.117710979560879,0.,-0.0461186027918559));
#7762=CARTESIAN_POINT('',(0.0721687836487032,-0.25,-0.125));
#7763=CARTESIAN_POINT('',(0.0721687836487032,0.,-0.125));
#7764=CARTESIAN_POINT('',(0.144337567297406,-0.25,0.));
#7765=CARTESIAN_POINT('',(0.144337567297406,-0.25,0.));
#7766=CARTESIAN_POINT('',(0.144337567297406,0.,0.));
#7767=CARTESIAN_POINT('Origin',(-0.0721687836487032,0.,-0.125));
#7768=CARTESIAN_POINT('',(-0.0721687836487032,0.,-0.125));
#7769=CARTESIAN_POINT('',(0.0739156081756484,0.,-0.125));
#7770=CARTESIAN_POINT('',(-0.0721687836487032,-0.25,-0.125));
#7771=CARTESIAN_POINT('',(-0.0721687836487032,0.,-0.125));
#7772=CARTESIAN_POINT('',(0.0721687836487032,-0.25,-0.125));
#7773=CARTESIAN_POINT('Origin',(-0.144337567297406,0.,-4.16333634234434E-17));
#7774=CARTESIAN_POINT('',(-0.144337567297406,0.,-1.76762539787485E-17));
#7775=CARTESIAN_POINT('',(-0.0987953713852306,0.,-0.0788813972081442));
#7776=CARTESIAN_POINT('',(-0.144337567297406,-0.25,-2.77555756156289E-17));
#7777=CARTESIAN_POINT('',(-0.144337567297406,0.,-1.76762539787485E-17));
#7778=CARTESIAN_POINT('',(-0.0721687836487032,-0.25,-0.125));
#7779=CARTESIAN_POINT('Origin',(-0.0721687836487033,0.,0.125));
#7780=CARTESIAN_POINT('',(-0.0721687836487033,0.,0.125));
#7781=CARTESIAN_POINT('',(-0.0627109795608791,0.,0.141381397208144));
#7782=CARTESIAN_POINT('',(-0.0721687836487033,-0.25,0.125));
#7783=CARTESIAN_POINT('',(-0.0721687836487033,0.,0.125));
#7784=CARTESIAN_POINT('',(-0.144337567297406,-0.25,-1.76762539787485E-17));
#7785=CARTESIAN_POINT('Origin',(0.0721687836487032,0.,0.125));
#7786=CARTESIAN_POINT('',(0.0721687836487032,0.,0.125));
#7787=CARTESIAN_POINT('',(0.146084391824352,0.,0.125));
#7788=CARTESIAN_POINT('',(0.0721687836487032,-0.25,0.125));
#7789=CARTESIAN_POINT('',(0.0721687836487032,0.,0.125));
#7790=CARTESIAN_POINT('',(-0.0721687836487033,-0.25,0.125));
#7791=CARTESIAN_POINT('Origin',(0.144337567297406,0.,0.));
#7792=CARTESIAN_POINT('',(0.153795371385231,0.,-0.0163813972081441));
#7793=CARTESIAN_POINT('',(0.0721687836487032,-0.25,0.125));
#7794=CARTESIAN_POINT('Origin',(0.,-0.25,0.));
#7795=CARTESIAN_POINT('Origin',(0.22,0.,0.));
#7796=CARTESIAN_POINT('',(-0.22,-8.67361737988404E-18,-2.69422295812418E-17));
#7797=CARTESIAN_POINT('Origin',(0.,0.,0.));
#7798=CARTESIAN_POINT('Origin',(0.,-0.015,0.));
#7799=CARTESIAN_POINT('',(-0.24505,-0.02505,-3.00099698131059E-17));
#7800=CARTESIAN_POINT('Origin',(0.,-0.02505,0.));
#7801=CARTESIAN_POINT('',(-0.235,-0.015,-2.87791997799628E-17));
#7802=CARTESIAN_POINT('Origin',(0.,-0.3775,0.));
#7803=CARTESIAN_POINT('',(-0.24505,-0.72995,3.00099698131059E-17));
#7804=CARTESIAN_POINT('Origin',(0.,-0.72995,0.));
#7805=CARTESIAN_POINT('',(-0.24505,-0.3775,-3.00099698131059E-17));
#7806=CARTESIAN_POINT('Origin',(0.,-0.7625,0.));
#7807=CARTESIAN_POINT('',(-0.175,-0.8,-2.14313189850787E-17));
#7808=CARTESIAN_POINT('Origin',(0.,-0.8,0.));
#7809=CARTESIAN_POINT('',(-0.2125,-0.7625,-2.60237444818813E-17));
#7810=CARTESIAN_POINT('Origin',(0.,-0.8,0.));
#7811=CARTESIAN_POINT('',(0.,0.,0.));
#7812=CARTESIAN_POINT('',(0.,0.,0.));
#7813=CARTESIAN_POINT('',(0.,0.,0.));
#7814=CARTESIAN_POINT('',(0.,0.,0.));
#7815=CARTESIAN_POINT('',(0.,6.4,6.3));
#7816=CARTESIAN_POINT('',(0.,-2.,3.85));
#7817=CARTESIAN_POINT('',(0.,-1.2,6.3));
#7818=CARTESIAN_POINT('',(0.,0.,0.));
#7819=CARTESIAN_POINT('',(0.,0.,0.));
#7820=UNCERTAINTY_MEASURE_WITH_UNIT(LENGTH_MEASURE(0.001),#7872,
'DISTANCE_ACCURACY_VALUE',
'Maximum model space distance between geometric entities at asserted c
onnectivities');
#7821=UNCERTAINTY_MEASURE_WITH_UNIT(LENGTH_MEASURE(0.001),#7872,
'DISTANCE_ACCURACY_VALUE',
'Maximum model space distance between geometric entities at asserted c
onnectivities');
#7822=UNCERTAINTY_MEASURE_WITH_UNIT(LENGTH_MEASURE(0.001),#7872,
'DISTANCE_ACCURACY_VALUE',
'Maximum model space distance between geometric entities at asserted c
onnectivities');
#7823=UNCERTAINTY_MEASURE_WITH_UNIT(LENGTH_MEASURE(0.001),#7872,
'DISTANCE_ACCURACY_VALUE',
'Maximum model space distance between geometric entities at asserted c
onnectivities');
#7824=UNCERTAINTY_MEASURE_WITH_UNIT(LENGTH_MEASURE(0.001),#7872,
'DISTANCE_ACCURACY_VALUE',
'Maximum model space distance between geometric entities at asserted c
onnectivities');
#7825=UNCERTAINTY_MEASURE_WITH_UNIT(LENGTH_MEASURE(0.001),#7872,
'DISTANCE_ACCURACY_VALUE',
'Maximum model space distance between geometric entities at asserted c
onnectivities');
#7826=UNCERTAINTY_MEASURE_WITH_UNIT(LENGTH_MEASURE(0.001),#7872,
'DISTANCE_ACCURACY_VALUE',
'Maximum model space distance between geometric entities at asserted c
onnectivities');
#7827=UNCERTAINTY_MEASURE_WITH_UNIT(LENGTH_MEASURE(0.001),#7872,
'DISTANCE_ACCURACY_VALUE',
'Maximum model space distance between geometric entities at asserted c
onnectivities');
#7828=UNCERTAINTY_MEASURE_WITH_UNIT(LENGTH_MEASURE(0.001),#7872,
'DISTANCE_ACCURACY_VALUE',
'Maximum model space distance between geometric entities at asserted c
onnectivities');
#7829=UNCERTAINTY_MEASURE_WITH_UNIT(LENGTH_MEASURE(0.001),#7872,
'DISTANCE_ACCURACY_VALUE',
'Maximum model space distance between geometric entities at asserted c
onnectivities');
#7830=UNCERTAINTY_MEASURE_WITH_UNIT(LENGTH_MEASURE(0.001),#7872,
'DISTANCE_ACCURACY_VALUE',
'Maximum model space distance between geometric entities at asserted c
onnectivities');
#7831=UNCERTAINTY_MEASURE_WITH_UNIT(LENGTH_MEASURE(0.001),#7872,
'DISTANCE_ACCURACY_VALUE',
'Maximum model space distance between geometric entities at asserted c
onnectivities');
#7832=UNCERTAINTY_MEASURE_WITH_UNIT(LENGTH_MEASURE(0.001),#7872,
'DISTANCE_ACCURACY_VALUE',
'Maximum model space distance between geometric entities at asserted c
onnectivities');
#7833=UNCERTAINTY_MEASURE_WITH_UNIT(LENGTH_MEASURE(0.001),#7872,
'DISTANCE_ACCURACY_VALUE',
'Maximum model space distance between geometric entities at asserted c
onnectivities');
#7834=UNCERTAINTY_MEASURE_WITH_UNIT(LENGTH_MEASURE(0.001),#7872,
'DISTANCE_ACCURACY_VALUE',
'Maximum model space distance between geometric entities at asserted c
onnectivities');
#7835=UNCERTAINTY_MEASURE_WITH_UNIT(LENGTH_MEASURE(0.001),#7872,
'DISTANCE_ACCURACY_VALUE',
'Maximum model space distance between geometric entities at asserted c
onnectivities');
#7836=UNCERTAINTY_MEASURE_WITH_UNIT(LENGTH_MEASURE(0.001),#7872,
'DISTANCE_ACCURACY_VALUE',
'Maximum model space distance between geometric entities at asserted c
onnectivities');
#7837=UNCERTAINTY_MEASURE_WITH_UNIT(LENGTH_MEASURE(0.001),#7872,
'DISTANCE_ACCURACY_VALUE',
'Maximum model space distance between geometric entities at asserted c
onnectivities');
#7838=UNCERTAINTY_MEASURE_WITH_UNIT(LENGTH_MEASURE(0.001),#7872,
'DISTANCE_ACCURACY_VALUE',
'Maximum model space distance between geometric entities at asserted c
onnectivities');
#7839=UNCERTAINTY_MEASURE_WITH_UNIT(LENGTH_MEASURE(0.001),#7872,
'DISTANCE_ACCURACY_VALUE',
'Maximum model space distance between geometric entities at asserted c
onnectivities');
#7840=UNCERTAINTY_MEASURE_WITH_UNIT(LENGTH_MEASURE(0.001),#7872,
'DISTANCE_ACCURACY_VALUE',
'Maximum model space distance between geometric entities at asserted c
onnectivities');
#7841=UNCERTAINTY_MEASURE_WITH_UNIT(LENGTH_MEASURE(0.001),#7872,
'DISTANCE_ACCURACY_VALUE',
'Maximum model space distance between geometric entities at asserted c
onnectivities');
#7842=UNCERTAINTY_MEASURE_WITH_UNIT(LENGTH_MEASURE(0.001),#7872,
'DISTANCE_ACCURACY_VALUE',
'Maximum model space distance between geometric entities at asserted c
onnectivities');
#7843=UNCERTAINTY_MEASURE_WITH_UNIT(LENGTH_MEASURE(0.001),#7872,
'DISTANCE_ACCURACY_VALUE',
'Maximum model space distance between geometric entities at asserted c
onnectivities');
#7844=UNCERTAINTY_MEASURE_WITH_UNIT(LENGTH_MEASURE(0.001),#7872,
'DISTANCE_ACCURACY_VALUE',
'Maximum model space distance between geometric entities at asserted c
onnectivities');
#7845=UNCERTAINTY_MEASURE_WITH_UNIT(LENGTH_MEASURE(0.001),#7872,
'DISTANCE_ACCURACY_VALUE',
'Maximum model space distance between geometric entities at asserted c
onnectivities');
#7846=(
GEOMETRIC_REPRESENTATION_CONTEXT(3)
GLOBAL_UNCERTAINTY_ASSIGNED_CONTEXT((#7820))
GLOBAL_UNIT_ASSIGNED_CONTEXT((#7872,#7874,#7875))
REPRESENTATION_CONTEXT('','3D')
);
#7847=(
GEOMETRIC_REPRESENTATION_CONTEXT(3)
GLOBAL_UNCERTAINTY_ASSIGNED_CONTEXT((#7821))
GLOBAL_UNIT_ASSIGNED_CONTEXT((#7872,#7874,#7875))
REPRESENTATION_CONTEXT('','3D')
);
#7848=(
GEOMETRIC_REPRESENTATION_CONTEXT(3)
GLOBAL_UNCERTAINTY_ASSIGNED_CONTEXT((#7822))
GLOBAL_UNIT_ASSIGNED_CONTEXT((#7872,#7874,#7875))
REPRESENTATION_CONTEXT('','3D')
);
#7849=(
GEOMETRIC_REPRESENTATION_CONTEXT(3)
GLOBAL_UNCERTAINTY_ASSIGNED_CONTEXT((#7823))
GLOBAL_UNIT_ASSIGNED_CONTEXT((#7872,#7874,#7875))
REPRESENTATION_CONTEXT('','3D')
);
#7850=(
GEOMETRIC_REPRESENTATION_CONTEXT(3)
GLOBAL_UNCERTAINTY_ASSIGNED_CONTEXT((#7824))
GLOBAL_UNIT_ASSIGNED_CONTEXT((#7872,#7874,#7875))
REPRESENTATION_CONTEXT('','3D')
);
#7851=(
GEOMETRIC_REPRESENTATION_CONTEXT(3)
GLOBAL_UNCERTAINTY_ASSIGNED_CONTEXT((#7825))
GLOBAL_UNIT_ASSIGNED_CONTEXT((#7872,#7874,#7875))
REPRESENTATION_CONTEXT('','3D')
);
#7852=(
GEOMETRIC_REPRESENTATION_CONTEXT(3)
GLOBAL_UNCERTAINTY_ASSIGNED_CONTEXT((#7826))
GLOBAL_UNIT_ASSIGNED_CONTEXT((#7872,#7874,#7875))
REPRESENTATION_CONTEXT('','3D')
);
#7853=(
GEOMETRIC_REPRESENTATION_CONTEXT(3)
GLOBAL_UNCERTAINTY_ASSIGNED_CONTEXT((#7827))
GLOBAL_UNIT_ASSIGNED_CONTEXT((#7872,#7874,#7875))
REPRESENTATION_CONTEXT('','3D')
);
#7854=(
GEOMETRIC_REPRESENTATION_CONTEXT(3)
GLOBAL_UNCERTAINTY_ASSIGNED_CONTEXT((#7828))
GLOBAL_UNIT_ASSIGNED_CONTEXT((#7872,#7874,#7875))
REPRESENTATION_CONTEXT('','3D')
);
#7855=(
GEOMETRIC_REPRESENTATION_CONTEXT(3)
GLOBAL_UNCERTAINTY_ASSIGNED_CONTEXT((#7829))
GLOBAL_UNIT_ASSIGNED_CONTEXT((#7872,#7874,#7875))
REPRESENTATION_CONTEXT('','3D')
);
#7856=(
GEOMETRIC_REPRESENTATION_CONTEXT(3)
GLOBAL_UNCERTAINTY_ASSIGNED_CONTEXT((#7830))
GLOBAL_UNIT_ASSIGNED_CONTEXT((#7872,#7874,#7875))
REPRESENTATION_CONTEXT('','3D')
);
#7857=(
GEOMETRIC_REPRESENTATION_CONTEXT(3)
GLOBAL_UNCERTAINTY_ASSIGNED_CONTEXT((#7831))
GLOBAL_UNIT_ASSIGNED_CONTEXT((#7872,#7874,#7875))
REPRESENTATION_CONTEXT('','3D')
);
#7858=(
GEOMETRIC_REPRESENTATION_CONTEXT(3)
GLOBAL_UNCERTAINTY_ASSIGNED_CONTEXT((#7832))
GLOBAL_UNIT_ASSIGNED_CONTEXT((#7872,#7874,#7875))
REPRESENTATION_CONTEXT('','3D')
);
#7859=(
GEOMETRIC_REPRESENTATION_CONTEXT(3)
GLOBAL_UNCERTAINTY_ASSIGNED_CONTEXT((#7833))
GLOBAL_UNIT_ASSIGNED_CONTEXT((#7872,#7874,#7875))
REPRESENTATION_CONTEXT('','3D')
);
#7860=(
GEOMETRIC_REPRESENTATION_CONTEXT(3)
GLOBAL_UNCERTAINTY_ASSIGNED_CONTEXT((#7834))
GLOBAL_UNIT_ASSIGNED_CONTEXT((#7872,#7874,#7875))
REPRESENTATION_CONTEXT('','3D')
);
#7861=(
GEOMETRIC_REPRESENTATION_CONTEXT(3)
GLOBAL_UNCERTAINTY_ASSIGNED_CONTEXT((#7835))
GLOBAL_UNIT_ASSIGNED_CONTEXT((#7872,#7874,#7875))
REPRESENTATION_CONTEXT('','3D')
);
#7862=(
GEOMETRIC_REPRESENTATION_CONTEXT(3)
GLOBAL_UNCERTAINTY_ASSIGNED_CONTEXT((#7836))
GLOBAL_UNIT_ASSIGNED_CONTEXT((#7872,#7874,#7875))
REPRESENTATION_CONTEXT('','3D')
);
#7863=(
GEOMETRIC_REPRESENTATION_CONTEXT(3)
GLOBAL_UNCERTAINTY_ASSIGNED_CONTEXT((#7837))
GLOBAL_UNIT_ASSIGNED_CONTEXT((#7872,#7874,#7875))
REPRESENTATION_CONTEXT('','3D')
);
#7864=(
GEOMETRIC_REPRESENTATION_CONTEXT(3)
GLOBAL_UNCERTAINTY_ASSIGNED_CONTEXT((#7838))
GLOBAL_UNIT_ASSIGNED_CONTEXT((#7872,#7874,#7875))
REPRESENTATION_CONTEXT('','3D')
);
#7865=(
GEOMETRIC_REPRESENTATION_CONTEXT(3)
GLOBAL_UNCERTAINTY_ASSIGNED_CONTEXT((#7839))
GLOBAL_UNIT_ASSIGNED_CONTEXT((#7872,#7874,#7875))
REPRESENTATION_CONTEXT('','3D')
);
#7866=(
GEOMETRIC_REPRESENTATION_CONTEXT(3)
GLOBAL_UNCERTAINTY_ASSIGNED_CONTEXT((#7840))
GLOBAL_UNIT_ASSIGNED_CONTEXT((#7872,#7874,#7875))
REPRESENTATION_CONTEXT('','3D')
);
#7867=(
GEOMETRIC_REPRESENTATION_CONTEXT(3)
GLOBAL_UNCERTAINTY_ASSIGNED_CONTEXT((#7841))
GLOBAL_UNIT_ASSIGNED_CONTEXT((#7872,#7874,#7875))
REPRESENTATION_CONTEXT('','3D')
);
#7868=(
GEOMETRIC_REPRESENTATION_CONTEXT(3)
GLOBAL_UNCERTAINTY_ASSIGNED_CONTEXT((#7842))
GLOBAL_UNIT_ASSIGNED_CONTEXT((#7872,#7874,#7875))
REPRESENTATION_CONTEXT('','3D')
);
#7869=(
GEOMETRIC_REPRESENTATION_CONTEXT(3)
GLOBAL_UNCERTAINTY_ASSIGNED_CONTEXT((#7843))
GLOBAL_UNIT_ASSIGNED_CONTEXT((#7872,#7874,#7875))
REPRESENTATION_CONTEXT('','3D')
);
#7870=(
GEOMETRIC_REPRESENTATION_CONTEXT(3)
GLOBAL_UNCERTAINTY_ASSIGNED_CONTEXT((#7844))
GLOBAL_UNIT_ASSIGNED_CONTEXT((#7872,#7874,#7875))
REPRESENTATION_CONTEXT('','3D')
);
#7871=(
GEOMETRIC_REPRESENTATION_CONTEXT(3)
GLOBAL_UNCERTAINTY_ASSIGNED_CONTEXT((#7845))
GLOBAL_UNIT_ASSIGNED_CONTEXT((#7872,#7874,#7875))
REPRESENTATION_CONTEXT('','3D')
);
#7872=(
LENGTH_UNIT()
NAMED_UNIT(*)
SI_UNIT(.CENTI.,.METRE.)
);
#7873=(
LENGTH_UNIT()
NAMED_UNIT(*)
SI_UNIT($,.METRE.)
);
#7874=(
NAMED_UNIT(*)
PLANE_ANGLE_UNIT()
SI_UNIT($,.RADIAN.)
);
#7875=(
NAMED_UNIT(*)
SI_UNIT($,.STERADIAN.)
SOLID_ANGLE_UNIT()
);
#7876=SHAPE_DEFINITION_REPRESENTATION(#7901,#7962);
#7877=SHAPE_DEFINITION_REPRESENTATION(#7902,#7963);
#7878=SHAPE_DEFINITION_REPRESENTATION(#7903,#7964);
#7879=SHAPE_DEFINITION_REPRESENTATION(#7904,#7965);
#7880=SHAPE_DEFINITION_REPRESENTATION(#7905,#7966);
#7881=SHAPE_DEFINITION_REPRESENTATION(#7906,#7967);
#7882=SHAPE_DEFINITION_REPRESENTATION(#7907,#7968);
#7883=SHAPE_DEFINITION_REPRESENTATION(#7908,#7969);
#7884=SHAPE_DEFINITION_REPRESENTATION(#7909,#7970);
#7885=SHAPE_DEFINITION_REPRESENTATION(#7910,#7971);
#7886=SHAPE_DEFINITION_REPRESENTATION(#7911,#7972);
#7887=SHAPE_DEFINITION_REPRESENTATION(#7912,#7973);
#7888=SHAPE_DEFINITION_REPRESENTATION(#7913,#7974);
#7889=SHAPE_DEFINITION_REPRESENTATION(#7914,#7975);
#7890=SHAPE_DEFINITION_REPRESENTATION(#7915,#7976);
#7891=SHAPE_DEFINITION_REPRESENTATION(#7916,#7977);
#7892=SHAPE_DEFINITION_REPRESENTATION(#7922,#7978);
#7893=SHAPE_DEFINITION_REPRESENTATION(#7923,#7979);
#7894=SHAPE_DEFINITION_REPRESENTATION(#7946,#7980);
#7895=SHAPE_DEFINITION_REPRESENTATION(#7947,#7981);
#7896=SHAPE_DEFINITION_REPRESENTATION(#7948,#7982);
#7897=SHAPE_DEFINITION_REPRESENTATION(#7949,#7983);
#7898=SHAPE_DEFINITION_REPRESENTATION(#7950,#7984);
#7899=SHAPE_DEFINITION_REPRESENTATION(#7951,#7985);
#7900=SHAPE_DEFINITION_REPRESENTATION(#7952,#7986);
#7901=PRODUCT_DEFINITION_SHAPE('',$,#7988);
#7902=PRODUCT_DEFINITION_SHAPE('',$,#7989);
#7903=PRODUCT_DEFINITION_SHAPE('',$,#7990);
#7904=PRODUCT_DEFINITION_SHAPE('',$,#7991);
#7905=PRODUCT_DEFINITION_SHAPE('',$,#7992);
#7906=PRODUCT_DEFINITION_SHAPE('',$,#7993);
#7907=PRODUCT_DEFINITION_SHAPE('',$,#7994);
#7908=PRODUCT_DEFINITION_SHAPE('',$,#7995);
#7909=PRODUCT_DEFINITION_SHAPE('',$,#7996);
#7910=PRODUCT_DEFINITION_SHAPE('',$,#7997);
#7911=PRODUCT_DEFINITION_SHAPE('',$,#7998);
#7912=PRODUCT_DEFINITION_SHAPE('',$,#7999);
#7913=PRODUCT_DEFINITION_SHAPE('',$,#8000);
#7914=PRODUCT_DEFINITION_SHAPE('',$,#8001);
#7915=PRODUCT_DEFINITION_SHAPE('',$,#8002);
#7916=PRODUCT_DEFINITION_SHAPE('',$,#8003);
#7917=PRODUCT_DEFINITION_SHAPE($,$,#123);
#7918=PRODUCT_DEFINITION_SHAPE($,$,#124);
#7919=PRODUCT_DEFINITION_SHAPE($,$,#125);
#7920=PRODUCT_DEFINITION_SHAPE($,$,#126);
#7921=PRODUCT_DEFINITION_SHAPE($,$,#127);
#7922=PRODUCT_DEFINITION_SHAPE('',$,#8004);
#7923=PRODUCT_DEFINITION_SHAPE('',$,#8005);
#7924=PRODUCT_DEFINITION_SHAPE($,$,#128);
#7925=PRODUCT_DEFINITION_SHAPE($,$,#129);
#7926=PRODUCT_DEFINITION_SHAPE($,$,#130);
#7927=PRODUCT_DEFINITION_SHAPE($,$,#131);
#7928=PRODUCT_DEFINITION_SHAPE($,$,#132);
#7929=PRODUCT_DEFINITION_SHAPE($,$,#133);
#7930=PRODUCT_DEFINITION_SHAPE($,$,#134);
#7931=PRODUCT_DEFINITION_SHAPE($,$,#135);
#7932=PRODUCT_DEFINITION_SHAPE($,$,#136);
#7933=PRODUCT_DEFINITION_SHAPE($,$,#137);
#7934=PRODUCT_DEFINITION_SHAPE($,$,#138);
#7935=PRODUCT_DEFINITION_SHAPE($,$,#139);
#7936=PRODUCT_DEFINITION_SHAPE($,$,#140);
#7937=PRODUCT_DEFINITION_SHAPE($,$,#141);
#7938=PRODUCT_DEFINITION_SHAPE($,$,#142);
#7939=PRODUCT_DEFINITION_SHAPE($,$,#143);
#7940=PRODUCT_DEFINITION_SHAPE($,$,#144);
#7941=PRODUCT_DEFINITION_SHAPE($,$,#145);
#7942=PRODUCT_DEFINITION_SHAPE($,$,#146);
#7943=PRODUCT_DEFINITION_SHAPE($,$,#147);
#7944=PRODUCT_DEFINITION_SHAPE($,$,#148);
#7945=PRODUCT_DEFINITION_SHAPE($,$,#149);
#7946=PRODUCT_DEFINITION_SHAPE('',$,#8006);
#7947=PRODUCT_DEFINITION_SHAPE('',$,#8007);
#7948=PRODUCT_DEFINITION_SHAPE('',$,#8008);
#7949=PRODUCT_DEFINITION_SHAPE('',$,#8009);
#7950=PRODUCT_DEFINITION_SHAPE('',$,#8010);
#7951=PRODUCT_DEFINITION_SHAPE('',$,#8011);
#7952=PRODUCT_DEFINITION_SHAPE('',$,#8012);
#7953=PRODUCT_DEFINITION_SHAPE($,$,#150);
#7954=PRODUCT_DEFINITION_SHAPE($,$,#151);
#7955=PRODUCT_DEFINITION_SHAPE($,$,#152);
#7956=PRODUCT_DEFINITION_SHAPE($,$,#153);
#7957=PRODUCT_DEFINITION_SHAPE($,$,#154);
#7958=PRODUCT_DEFINITION_SHAPE($,$,#155);
#7959=PRODUCT_DEFINITION_SHAPE($,$,#156);
#7960=PRODUCT_DEFINITION_SHAPE($,$,#157);
#7961=PRODUCT_DEFINITION_SHAPE($,$,#158);
#7962=SHAPE_REPRESENTATION('',(#4348,#4878,#4879),#7846);
#7963=SHAPE_REPRESENTATION('',(#4349,#4741,#4742,#4743,#4744,#4745,#4746,
#4747,#4748,#4749,#4750,#4751,#4752,#4753,#4754,#4755,#4756,#4757,#4758,
#4759,#4760,#4761,#4762),#7847);
#7964=SHAPE_REPRESENTATION('',(#4350),#7848);
#7965=SHAPE_REPRESENTATION('',(#4369),#7849);
#7966=SHAPE_REPRESENTATION('',(#4448),#7850);
#7967=SHAPE_REPRESENTATION('',(#4457),#7851);
#7968=SHAPE_REPRESENTATION('',(#4486),#7852);
#7969=SHAPE_REPRESENTATION('',(#4495),#7853);
#7970=SHAPE_REPRESENTATION('',(#4541),#7854);
#7971=SHAPE_REPRESENTATION('',(#4548),#7855);
#7972=SHAPE_REPRESENTATION('',(#4555,#4684,#4685,#4686,#4687,#4688),#7856);
#7973=SHAPE_REPRESENTATION('',(#4556),#7857);
#7974=SHAPE_REPRESENTATION('',(#4576),#7858);
#7975=SHAPE_REPRESENTATION('',(#4596),#7859);
#7976=SHAPE_REPRESENTATION('',(#4613),#7860);
#7977=SHAPE_REPRESENTATION('',(#4667),#7861);
#7978=SHAPE_REPRESENTATION('',(#4689),#7862);
#7979=SHAPE_REPRESENTATION('',(#4715),#7863);
#7980=SHAPE_REPRESENTATION('',(#4763,#4871,#4872,#4873,#4874,#4875,#4876,
#4877),#7864);
#7981=SHAPE_REPRESENTATION('',(#4764),#7865);
#7982=SHAPE_REPRESENTATION('',(#4785),#7866);
#7983=SHAPE_REPRESENTATION('',(#4794),#7867);
#7984=SHAPE_REPRESENTATION('',(#4809),#7868);
#7985=SHAPE_REPRESENTATION('',(#4843),#7869);
#7986=SHAPE_REPRESENTATION('',(#4854),#7870);
#7987=PRODUCT_DEFINITION_CONTEXT('part definition',#8064,'design');
#7988=PRODUCT_DEFINITION('PAT-008',
'PAT-008',#8013,#7987);
#7989=PRODUCT_DEFINITION('Bearing housing','Bearing housing',#8014,#7987);
#7990=PRODUCT_DEFINITION('Base','Base',#8015,#7987);
#7991=PRODUCT_DEFINITION('Housing','Housing',#8016,#7987);
#7992=PRODUCT_DEFINITION('Outer race spacer','Outer race spacer',#8017,
#7987);
#7993=PRODUCT_DEFINITION('Seal cap','Seal cap',#8018,#7987);
#7994=PRODUCT_DEFINITION('Dust seal envelope','Dust seal envelope',#8019,
#7987);
#7995=PRODUCT_DEFINITION('Blind cap','Blind cap',#8020,#7987);
#7996=PRODUCT_DEFINITION('Bonded base pad','Bonded base pad',#8021,#7987);
#7997=PRODUCT_DEFINITION('Bonded base pad (1)','Bonded base pad (1)',#8022,
#7987);
#7998=PRODUCT_DEFINITION('Sealed Ball Bearing - 20 x 47 x 14 mm',
'Sealed Ball Bearing - 20 x 47 x 14 mm',#8023,#7987);
#7999=PRODUCT_DEFINITION('Inner ring','Inner ring',#8024,#7987);
#8000=PRODUCT_DEFINITION('Outer ring','Outer ring',#8025,#7987);
#8001=PRODUCT_DEFINITION('Balls','Balls',#8026,#7987);
#8002=PRODUCT_DEFINITION('Cage','Cage',#8027,#7987);
#8003=PRODUCT_DEFINITION('Seals 2RS','Seals 2RS',#8028,#7987);
#8004=PRODUCT_DEFINITION('Cap Screw - M6x25','Cap Screw - M6x25',#8029,
#7987);
#8005=PRODUCT_DEFINITION('Cap Screw - M4x16','Cap Screw - M4x16',#8030,
#7987);
#8006=PRODUCT_DEFINITION('Shaft and drive','Shaft and drive',#8031,#7987);
#8007=PRODUCT_DEFINITION('Stepped shaft','Stepped shaft',#8032,#7987);
#8008=PRODUCT_DEFINITION('Inner race spacer','Inner race spacer',#8033,
#7987);
#8009=PRODUCT_DEFINITION('Shaft collar','Shaft collar',#8034,#7987);
#8010=PRODUCT_DEFINITION('Drive flange','Drive flange',#8035,#7987);
#8011=PRODUCT_DEFINITION('Key 6x6x20','Key 6x6x20',#8036,#7987);
#8012=PRODUCT_DEFINITION('Socket Set Screw - M5x8',
'Socket Set Screw - M5x8',#8037,#7987);
#8013=PRODUCT_DEFINITION_FORMATION('',$,#8066);
#8014=PRODUCT_DEFINITION_FORMATION('',$,#8067);
#8015=PRODUCT_DEFINITION_FORMATION('',$,#8068);
#8016=PRODUCT_DEFINITION_FORMATION('',$,#8069);
#8017=PRODUCT_DEFINITION_FORMATION('',$,#8070);
#8018=PRODUCT_DEFINITION_FORMATION('',$,#8071);
#8019=PRODUCT_DEFINITION_FORMATION('',$,#8072);
#8020=PRODUCT_DEFINITION_FORMATION('',$,#8073);
#8021=PRODUCT_DEFINITION_FORMATION('',$,#8074);
#8022=PRODUCT_DEFINITION_FORMATION('',$,#8075);
#8023=PRODUCT_DEFINITION_FORMATION('',$,#8076);
#8024=PRODUCT_DEFINITION_FORMATION('',$,#8077);
#8025=PRODUCT_DEFINITION_FORMATION('',$,#8078);
#8026=PRODUCT_DEFINITION_FORMATION('',$,#8079);
#8027=PRODUCT_DEFINITION_FORMATION('',$,#8080);
#8028=PRODUCT_DEFINITION_FORMATION('',$,#8081);
#8029=PRODUCT_DEFINITION_FORMATION('',$,#8082);
#8030=PRODUCT_DEFINITION_FORMATION('',$,#8083);
#8031=PRODUCT_DEFINITION_FORMATION('',$,#8084);
#8032=PRODUCT_DEFINITION_FORMATION('',$,#8085);
#8033=PRODUCT_DEFINITION_FORMATION('',$,#8086);
#8034=PRODUCT_DEFINITION_FORMATION('',$,#8087);
#8035=PRODUCT_DEFINITION_FORMATION('',$,#8088);
#8036=PRODUCT_DEFINITION_FORMATION('',$,#8089);
#8037=PRODUCT_DEFINITION_FORMATION('',$,#8090);
#8038=PRODUCT_RELATED_PRODUCT_CATEGORY('PAT-008','PAT-008',(#8066));
#8039=PRODUCT_RELATED_PRODUCT_CATEGORY('Bearing housing',
'Bearing housing',(#8067));
#8040=PRODUCT_RELATED_PRODUCT_CATEGORY('Base','Base',(#8068));
#8041=PRODUCT_RELATED_PRODUCT_CATEGORY('Housing','Housing',(#8069));
#8042=PRODUCT_RELATED_PRODUCT_CATEGORY('Outer race spacer',
'Outer race spacer',(#8070));
#8043=PRODUCT_RELATED_PRODUCT_CATEGORY('Seal cap','Seal cap',(#8071));
#8044=PRODUCT_RELATED_PRODUCT_CATEGORY('Dust seal envelope',
'Dust seal envelope',(#8072));
#8045=PRODUCT_RELATED_PRODUCT_CATEGORY('Blind cap','Blind cap',(#8073));
#8046=PRODUCT_RELATED_PRODUCT_CATEGORY('Bonded base pad',
'Bonded base pad',(#8074));
#8047=PRODUCT_RELATED_PRODUCT_CATEGORY('Bonded base pad (1)',
'Bonded base pad (1)',(#8075));
#8048=PRODUCT_RELATED_PRODUCT_CATEGORY(
'Sealed Ball Bearing - 20 x 47 x 14 mm',
'Sealed Ball Bearing - 20 x 47 x 14 mm',(#8076));
#8049=PRODUCT_RELATED_PRODUCT_CATEGORY('Inner ring','Inner ring',(#8077));
#8050=PRODUCT_RELATED_PRODUCT_CATEGORY('Outer ring','Outer ring',(#8078));
#8051=PRODUCT_RELATED_PRODUCT_CATEGORY('Balls','Balls',(#8079));
#8052=PRODUCT_RELATED_PRODUCT_CATEGORY('Cage','Cage',(#8080));
#8053=PRODUCT_RELATED_PRODUCT_CATEGORY('Seals 2RS','Seals 2RS',(#8081));
#8054=PRODUCT_RELATED_PRODUCT_CATEGORY('Cap Screw - M6x25',
'Cap Screw - M6x25',(#8082));
#8055=PRODUCT_RELATED_PRODUCT_CATEGORY('Cap Screw - M4x16',
'Cap Screw - M4x16',(#8083));
#8056=PRODUCT_RELATED_PRODUCT_CATEGORY('Shaft and drive',
'Shaft and drive',(#8084));
#8057=PRODUCT_RELATED_PRODUCT_CATEGORY('Stepped shaft','Stepped shaft',
(#8085));
#8058=PRODUCT_RELATED_PRODUCT_CATEGORY('Inner race spacer',
'Inner race spacer',(#8086));
#8059=PRODUCT_RELATED_PRODUCT_CATEGORY('Shaft collar','Shaft collar',(#8087));
#8060=PRODUCT_RELATED_PRODUCT_CATEGORY('Drive flange','Drive flange',(#8088));
#8061=PRODUCT_RELATED_PRODUCT_CATEGORY('Key 6x6x20','Key 6x6x20',(#8089));
#8062=PRODUCT_RELATED_PRODUCT_CATEGORY('Socket Set Screw - M5x8',
'Socket Set Screw - M5x8',(#8090));
#8063=APPLICATION_PROTOCOL_DEFINITION('international standard',
'automotive_design',2009,#8064);
#8064=APPLICATION_CONTEXT(
'Core Data for Automotive Mechanical Design Process');
#8065=PRODUCT_CONTEXT('part definition',#8064,'mechanical');
#8066=PRODUCT('PAT-008','PAT-008',
'PAT-008',(#8065));
#8067=PRODUCT('Bearing housing','Bearing housing','Bearing housing',(#8065));
#8068=PRODUCT('Base','Base','Base',(#8065));
#8069=PRODUCT('Housing','Housing','Housing',(#8065));
#8070=PRODUCT('Outer race spacer','Outer race spacer',
'Outer race spacer',(#8065));
#8071=PRODUCT('Seal cap','Seal cap','Seal cap',(#8065));
#8072=PRODUCT('Dust seal envelope','Dust seal envelope',
'Dust seal envelope',(#8065));
#8073=PRODUCT('Blind cap','Blind cap','Blind cap',(#8065));
#8074=PRODUCT('Bonded base pad','Bonded base pad','Bonded base pad',(#8065));
#8075=PRODUCT('Bonded base pad (1)','Bonded base pad (1)',
'Bonded base pad (1)',(#8065));
#8076=PRODUCT('Sealed Ball Bearing - 20 x 47 x 14 mm',
'Sealed Ball Bearing - 20 x 47 x 14 mm',
'Sealed Ball Bearing - 20 x 47 x 14 mm',(#8065));
#8077=PRODUCT('Inner ring','Inner ring','Inner ring',(#8065));
#8078=PRODUCT('Outer ring','Outer ring','Outer ring',(#8065));
#8079=PRODUCT('Balls','Balls','Balls',(#8065));
#8080=PRODUCT('Cage','Cage','Cage',(#8065));
#8081=PRODUCT('Seals 2RS','Seals 2RS','Seals 2RS',(#8065));
#8082=PRODUCT('Cap Screw - M6x25','Cap Screw - M6x25',
'Cap Screw - M6x25',(#8065));
#8083=PRODUCT('Cap Screw - M4x16','Cap Screw - M4x16',
'Cap Screw - M4x16',(#8065));
#8084=PRODUCT('Shaft and drive','Shaft and drive','Shaft and drive',(#8065));
#8085=PRODUCT('Stepped shaft','Stepped shaft','Stepped shaft',(#8065));
#8086=PRODUCT('Inner race spacer','Inner race spacer',
'Inner race spacer',(#8065));
#8087=PRODUCT('Shaft collar','Shaft collar','Shaft collar',(#8065));
#8088=PRODUCT('Drive flange','Drive flange','Drive flange',(#8065));
#8089=PRODUCT('Key 6x6x20','Key 6x6x20','Key 6x6x20',(#8065));
#8090=PRODUCT('Socket Set Screw - M5x8','Socket Set Screw - M5x8',
'Socket Set Screw - M5x8',(#8065));
#8091=PRESENTATION_STYLE_ASSIGNMENT((#8096));
#8092=PRESENTATION_STYLE_ASSIGNMENT((#8097));
#8093=PRESENTATION_STYLE_ASSIGNMENT((#8098));
#8094=PRESENTATION_STYLE_ASSIGNMENT((#8099));
#8095=PRESENTATION_STYLE_ASSIGNMENT((#8100));
#8096=SURFACE_STYLE_USAGE(.BOTH.,#8101);
#8097=SURFACE_STYLE_USAGE(.BOTH.,#8102);
#8098=SURFACE_STYLE_USAGE(.BOTH.,#8103);
#8099=SURFACE_STYLE_USAGE(.BOTH.,#8104);
#8100=SURFACE_STYLE_USAGE(.BOTH.,#8105);
#8101=SURFACE_SIDE_STYLE('',(#8106));
#8102=SURFACE_SIDE_STYLE('',(#8107));
#8103=SURFACE_SIDE_STYLE('',(#8108));
#8104=SURFACE_SIDE_STYLE('',(#8109));
#8105=SURFACE_SIDE_STYLE('',(#8110));
#8106=SURFACE_STYLE_FILL_AREA(#8111);
#8107=SURFACE_STYLE_FILL_AREA(#8112);
#8108=SURFACE_STYLE_FILL_AREA(#8113);
#8109=SURFACE_STYLE_FILL_AREA(#8114);
#8110=SURFACE_STYLE_FILL_AREA(#8115);
#8111=FILL_AREA_STYLE('Steel - Satin',(#8116));
#8112=FILL_AREA_STYLE('CAD Library Painted - Deep blue',(#8117));
#8113=FILL_AREA_STYLE('CAD Library Painted - Engineering blue',(#8118));
#8114=FILL_AREA_STYLE('CAD Library Painted - Steel gray',(#8119));
#8115=FILL_AREA_STYLE('CAD Library Painted - Graphite',(#8120));
#8116=FILL_AREA_STYLE_COLOUR('Steel - Satin',#8121);
#8117=FILL_AREA_STYLE_COLOUR('CAD Library Painted - Deep blue',#8122);
#8118=FILL_AREA_STYLE_COLOUR('CAD Library Painted - Engineering blue',#8123);
#8119=FILL_AREA_STYLE_COLOUR('CAD Library Painted - Steel gray',#8124);
#8120=FILL_AREA_STYLE_COLOUR('CAD Library Painted - Graphite',#8125);
#8121=COLOUR_RGB('Steel - Satin',0.627450980392157,0.627450980392157,0.627450980392157);
#8122=COLOUR_RGB('CAD Library Painted - Deep blue',0.0784313725490196,0.203921568627451,
0.349019607843137);
#8123=COLOUR_RGB('CAD Library Painted - Engineering blue',0.12156862745098,
0.356862745098039,0.6);
#8124=COLOUR_RGB('CAD Library Painted - Steel gray',0.592156862745098,0.631372549019608,
0.67843137254902);
#8125=COLOUR_RGB('CAD Library Painted - Graphite',0.168627450980392,0.192156862745098,
0.231372549019608);
#8126=COLOUR_RGB('Dark Blue',0.08,0.2,0.34);
#8127=FILL_AREA_STYLE_COLOUR('',#8126);
#8128=FILL_AREA_STYLE('',(#8127));
#8129=SURFACE_STYLE_FILL_AREA(#8128);
#8130=SURFACE_SIDE_STYLE('',(#8129));
#8131=SURFACE_STYLE_USAGE(.BOTH.,#8130);
#8132=PRESENTATION_STYLE_ASSIGNMENT((#8131));
#8133=COLOUR_RGB('Light Blue',0.38,0.62,0.78);
#8134=FILL_AREA_STYLE_COLOUR('',#8133);
#8135=FILL_AREA_STYLE('',(#8134));
#8136=SURFACE_STYLE_FILL_AREA(#8135);
#8137=SURFACE_SIDE_STYLE('',(#8136));
#8138=SURFACE_STYLE_USAGE(.BOTH.,#8137);
#8139=PRESENTATION_STYLE_ASSIGNMENT((#8138));
#8140=COLOUR_RGB('Sky Blue',0.24,0.69,0.87);
#8141=FILL_AREA_STYLE_COLOUR('',#8140);
#8142=FILL_AREA_STYLE('',(#8141));
#8143=SURFACE_STYLE_FILL_AREA(#8142);
#8144=SURFACE_SIDE_STYLE('',(#8143));
#8145=SURFACE_STYLE_USAGE(.BOTH.,#8144);
#8146=PRESENTATION_STYLE_ASSIGNMENT((#8145));
#8147=COLOUR_RGB('Grey',0.48,0.52,0.57);
#8148=FILL_AREA_STYLE_COLOUR('',#8147);
#8149=FILL_AREA_STYLE('',(#8148));
#8150=SURFACE_STYLE_FILL_AREA(#8149);
#8151=SURFACE_SIDE_STYLE('',(#8150));
#8152=SURFACE_STYLE_USAGE(.BOTH.,#8151);
#8153=PRESENTATION_STYLE_ASSIGNMENT((#8152));
#8154=COLOUR_RGB('Black',0.12,0.14,0.17);
#8155=FILL_AREA_STYLE_COLOUR('',#8154);
#8156=FILL_AREA_STYLE('',(#8155));
#8157=SURFACE_STYLE_FILL_AREA(#8156);
#8158=SURFACE_SIDE_STYLE('',(#8157));
#8159=SURFACE_STYLE_USAGE(.BOTH.,#8158);
#8160=PRESENTATION_STYLE_ASSIGNMENT((#8159));
#8161=COLOUR_RGB('Off White',0.89,0.88,0.83);
#8162=FILL_AREA_STYLE_COLOUR('',#8161);
#8163=FILL_AREA_STYLE('',(#8162));
#8164=SURFACE_STYLE_FILL_AREA(#8163);
#8165=SURFACE_SIDE_STYLE('',(#8164));
#8166=SURFACE_STYLE_USAGE(.BOTH.,#8165);
#8167=PRESENTATION_STYLE_ASSIGNMENT((#8166));
ENDSEC;
END-ISO-10303-21;
